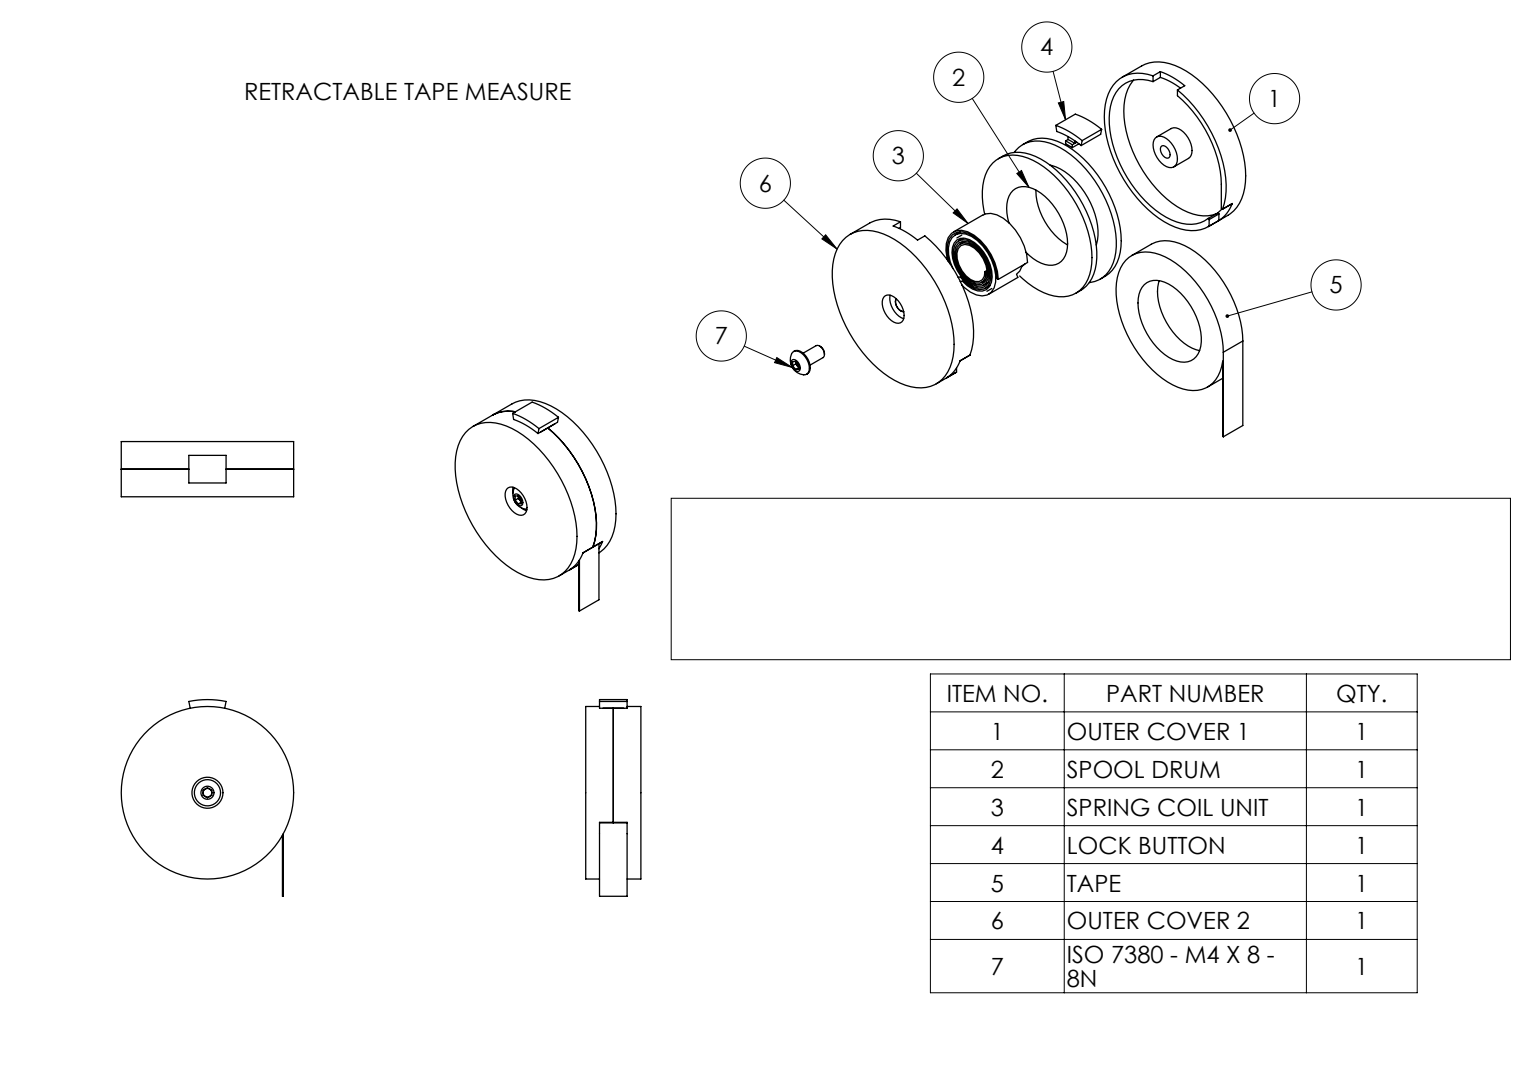
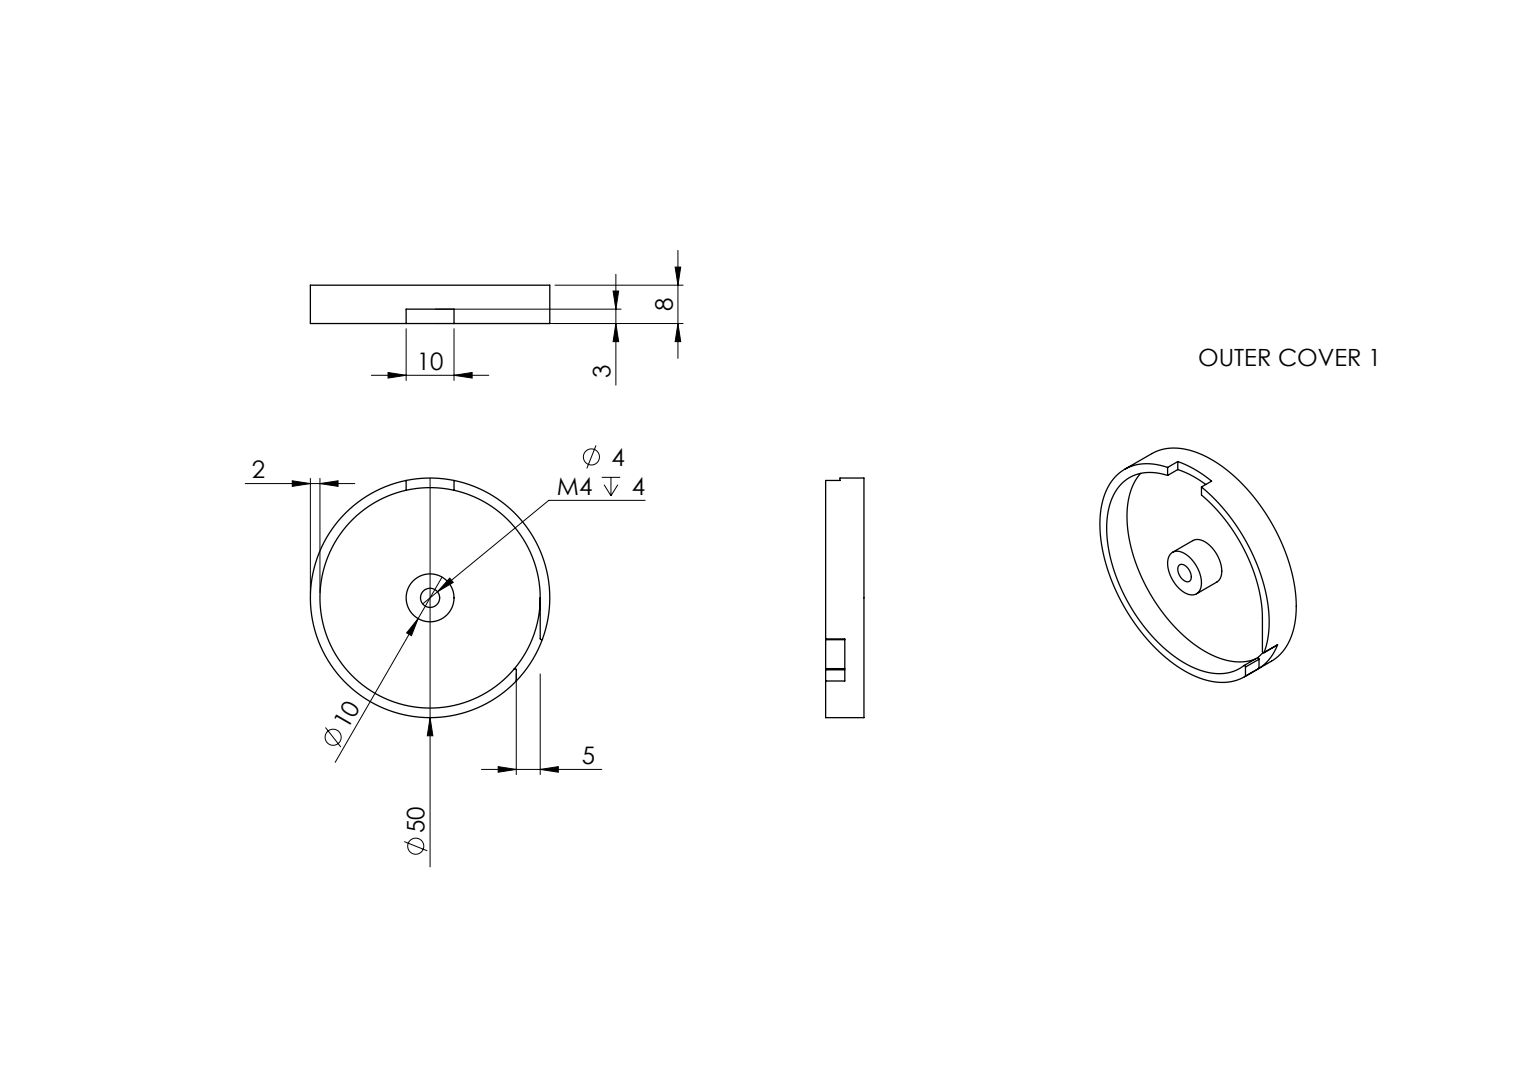
ISO-10303-21;
HEADER;
FILE_DESCRIPTION (('STEP AP214'),
    '1' );
FILE_NAME ('TAS-001',
    '2026-10-23T14:45:25',
    ( '' ),
    ( '' ),
    'SwSTEP 2.0',
    'SolidWorks 2026',
    '' );
FILE_SCHEMA (( 'AUTOMOTIVE_DESIGN' ));
ENDSEC;

DATA;
#1 = CARTESIAN_POINT ( 'NONE',  ( -5.525185448606692695, 2.707100724334796649, 1.999999999999998224 ) ) ;
#2 = DIRECTION ( 'NONE',  ( -1.000000000000000000, 0.000000000000000000, 0.000000000000000000 ) ) ;
#3 = ORIENTED_EDGE ( 'NONE', *, *, #653, .T. ) ;
#4 = EDGE_CURVE ( 'NONE', #1240, #2861, #1350, .T. ) ;
#5 = CARTESIAN_POINT ( 'NONE',  ( 10.20000000000000107, 1.971681346627238735E-16, -1.610000000000000098 ) ) ;
#6 = EDGE_CURVE ( 'NONE', #2459, #3011, #3096, .T. ) ;
#7 = CARTESIAN_POINT ( 'NONE',  ( 10.06493078320225010, 4.366638945734137245, 13.99999999999999645 ) ) ;
#8 = FILL_AREA_STYLE ('',( #407 ) ) ;
#9 = ORIENTED_EDGE ( 'NONE', *, *, #93, .F. ) ;
#10 = FACE_OUTER_BOUND ( 'NONE', #593, .T. ) ;
#11 = VERTEX_POINT ( 'NONE', #3151 ) ;
#12 = EDGE_LOOP ( 'NONE', ( #4243, #1543, #1314, #4388, #708 ) ) ;
#13 = CARTESIAN_POINT ( 'NONE',  ( 8.453438707197836521, 0.9797652757261499090, 14.00000000000000000 ) ) ;
#14 = CARTESIAN_POINT ( 'NONE',  ( 3.892125705850321804, -6.036954802193386982, 1.999999999999998224 ) ) ;
#15 = FACE_OUTER_BOUND ( 'NONE', #2318, .T. ) ;
#16 = CARTESIAN_POINT ( 'NONE',  ( 7.990059919442007441, -3.149571442993018167, 14.00000000000000000 ) ) ;
#17 = ORIENTED_EDGE ( 'NONE', *, *, #5283, .F. ) ;
#18 = CARTESIAN_POINT ( 'NONE',  ( -2.440069559021881496, 10.46881825416662259, 1.999999999999998224 ) ) ;
#19 = CARTESIAN_POINT ( 'NONE',  ( -5.000000000000085265, 24.49489742783176638, 8.000000000000000000 ) ) ;
#20 = CARTESIAN_POINT ( 'NONE',  ( 5.887534416617372202, 3.663839002572494952, 13.99999999999999645 ) ) ;
#21 = DIRECTION ( 'NONE',  ( 1.000000000000000000, 0.000000000000000000, 0.000000000000000000 ) ) ;
#22 = CARTESIAN_POINT ( 'NONE',  ( -2.415560149437878668, -8.486491385245608754, 1.999999999999998224 ) ) ;
#23 = EDGE_CURVE ( 'NONE', #5658, #4842, #4898, .T. ) ;
#24 = CARTESIAN_POINT ( 'NONE',  ( 2.877506500681688006, 7.288437455188073955, 1.999999999999998224 ) ) ;
#25 = LINE ( 'NONE', #396, #4267 ) ;
#26 = FILL_AREA_STYLE ('',( #3055 ) ) ;
#27 = DIRECTION ( 'NONE',  ( 0.000000000000000000, 0.000000000000000000, -1.000000000000000000 ) ) ;
#28 = FACE_OUTER_BOUND ( 'NONE', #3065, .T. ) ;
#29 = CARTESIAN_POINT ( 'NONE',  ( -25.00000000000000000, 0.000000000000000000, -8.000000000000000000 ) ) ;
#30 = VERTEX_POINT ( 'NONE', #94 ) ;
#31 = DIRECTION ( 'NONE',  ( -1.000000000000000000, 0.000000000000000000, 0.000000000000000000 ) ) ;
#32 = CARTESIAN_POINT ( 'NONE',  ( -10.48421140591525713, 1.206973991593908169, 13.99999999999999645 ) ) ;
#33 = AXIS2_PLACEMENT_3D ( 'NONE', #3461, #5223, #4408 ) ;
#34 = DIRECTION ( 'NONE',  ( 0.000000000000000000, 0.000000000000000000, -1.000000000000000000 ) ) ;
#35 = DIRECTION ( 'NONE',  ( 1.000000000000000000, 0.000000000000000000, -0.000000000000000000 ) ) ;
#36 = VERTEX_POINT ( 'NONE', #2452 ) ;
#37 = ORIENTED_EDGE ( 'NONE', *, *, #2017, .F. ) ;
#38 = CARTESIAN_POINT ( 'NONE',  ( -0.2798806129217078498, -8.779921314117062892, 14.00000000000000000 ) ) ;
#39 = CARTESIAN_POINT ( 'NONE',  ( 6.444084565535371567, 4.617298776321547393, 1.999999999999998224 ) ) ;
#40 = CIRCLE ( 'NONE', #4910, 25.00000000000000000 ) ;
#41 = DIRECTION ( 'NONE',  ( -0.000000000000000000, -0.000000000000000000, 1.000000000000000000 ) ) ;
#42 = CARTESIAN_POINT ( 'NONE',  ( -2.415560149437796511, -8.486491385245610530, 14.00000000000000000 ) ) ;
#43 = CIRCLE ( 'NONE', #2159, 23.00000000000000000 ) ;
#44 = ORIENTED_EDGE ( 'NONE', *, *, #3966, .F. ) ;
#45 = CARTESIAN_POINT ( 'NONE',  ( 8.595497693523489247, -5.345940745659027549, 1.999999999999998224 ) ) ;
#46 = CARTESIAN_POINT ( 'NONE',  ( -5.651290410005069376, 9.082320918485367045, 1.999999999999998224 ) ) ;
#47 =( GEOMETRIC_REPRESENTATION_CONTEXT ( 3 ) GLOBAL_UNCERTAINTY_ASSIGNED_CONTEXT ( ( #114 ) ) GLOBAL_UNIT_ASSIGNED_CONTEXT ( ( #3594, #2760, #4052 ) ) REPRESENTATION_CONTEXT ( 'NONE', 'WORKASPACE' ) );
#48 = CARTESIAN_POINT ( 'NONE',  ( -1.424809953814591523, 6.586142414399822620, 13.99999999999999645 ) ) ;
#49 = CARTESIAN_POINT ( 'NONE',  ( 7.716263785693136867, -3.801003699432787375, 1.999999999999998224 ) ) ;
#50 = CIRCLE ( 'NONE', #4195, 0.2500000000000002220 ) ;
#51 = CARTESIAN_POINT ( 'NONE',  ( 6.638644669766898154, 2.135480210976827387, 1.999999999999998224 ) ) ;
#52 = FILL_AREA_STYLE_COLOUR ( '', #5106 ) ;
#53 = DIRECTION ( 'NONE',  ( -0.000000000000000000, -0.000000000000000000, -1.000000000000000000 ) ) ;
#54 = VECTOR ( 'NONE', #1585, 1000.000000000000000 ) ;
#55 = CARTESIAN_POINT ( 'NONE',  ( 1.380000000000002336, 22.95856267278071172, 12.00000000000000000 ) ) ;
#56 = CARTESIAN_POINT ( 'NONE',  ( 2.199999999999999289, 0.000000000000000000, -3.300000000000000266 ) ) ;
#57 = CARTESIAN_POINT ( 'NONE',  ( -23.00000000000000000, 0.000000000000000000, 8.000000000000000000 ) ) ;
#58 = EDGE_LOOP ( 'NONE', ( #1044, #3800, #158, #292 ) ) ;
#59 = COLOUR_RGB ( '',0.8941176470588234615, 0.8941176470588234615, 0.8941176470588234615 ) ;
#60 = DIRECTION ( 'NONE',  ( -0.7071067811865492381, 8.659560562354911904E-17, -0.7071067811865457964 ) ) ;
#61 = CARTESIAN_POINT ( 'NONE',  ( -3.798941939731700579, -9.621416145859109648, 13.99999999999999645 ) ) ;
#62 = FILL_AREA_STYLE_COLOUR ( '', #2698 ) ;
#63 = CARTESIAN_POINT ( 'NONE',  ( -12.50000000000000000, 0.000000000000000000, 14.00000000000000000 ) ) ;
#64 = ORIENTED_EDGE ( 'NONE', *, *, #3045, .T. ) ;
#65 = ORIENTED_EDGE ( 'NONE', *, *, #4214, .F. ) ;
#66 = CARTESIAN_POINT ( 'NONE',  ( -7.161907081466633684, 5.673982509929174967, 14.00000000000000000 ) ) ;
#67 = CARTESIAN_POINT ( 'NONE',  ( 7.024953159363688471, -4.052930060063556716, 1.999999999999998224 ) ) ;
#68 = AXIS2_PLACEMENT_3D ( 'NONE', #3117, #2273, #3510 ) ;
#69 = ADVANCED_BREP_SHAPE_REPRESENTATION ( '', ( #652, #1336 ), #2338 ) ;
#70 = CARTESIAN_POINT ( 'NONE',  ( -7.550296695603107899, -2.566425989403007257, 1.999999999999998224 ) ) ;
#71 = CARTESIAN_POINT ( 'NONE',  ( 0.7514524083000287957, 9.263466152293682754, 14.00000000000000000 ) ) ;
#72 = VECTOR ( 'NONE', #3186, 1000.000000000000000 ) ;
#73 = VERTEX_POINT ( 'NONE', #3260 ) ;
#74 = CARTESIAN_POINT ( 'NONE',  ( 9.807503887220748950, -2.283819133639664489, 1.999999999999998224 ) ) ;
#75 = CARTESIAN_POINT ( 'NONE',  ( 6.160418207306094018, 1.983851483784787373, 14.00000000000000000 ) ) ;
#76 = CARTESIAN_POINT ( 'NONE',  ( -7.091148812992124739, -4.571561645351811976, 13.99999999999999645 ) ) ;
#77 = CARTESIAN_POINT ( 'NONE',  ( -8.026550172065741506, -2.724140490265046122, 13.99999999999999645 ) ) ;
#78 = ITEM_DEFINED_TRANSFORMATION ( 'NONE', 'NONE', #1407,  #1336 ) ;
#79 = CARTESIAN_POINT ( 'NONE',  ( -4.424777426321968576, -7.679192617323552739, 1.999999999999998224 ) ) ;
#80 = CARTESIAN_POINT ( 'NONE',  ( 5.887534416617370425, 3.663839002572738313, 1.999999999999998224 ) ) ;
#81 = EDGE_CURVE ( 'NONE', #5595, #92, #3920, .T. ) ;
#82 = CARTESIAN_POINT ( 'NONE',  ( -2.149999999999997691, 2.632990618166807263E-16, -8.000000000000000000 ) ) ;
#83 =( NAMED_UNIT ( * ) SI_UNIT ( $, .STERADIAN. ) SOLID_ANGLE_UNIT ( ) );
#84 = CARTESIAN_POINT ( 'NONE',  ( 1.380000000000002558, 22.95856267278071527, 1.371299631966804711 ) ) ;
#85 = DIRECTION ( 'NONE',  ( 0.000000000000000000, 0.000000000000000000, 1.000000000000000000 ) ) ;
#86 = FACE_OUTER_BOUND ( 'NONE', #1906, .T. ) ;
#87 = DIRECTION ( 'NONE',  ( 0.000000000000000000, 0.000000000000000000, -1.000000000000000000 ) ) ;
#88 = ADVANCED_FACE ( 'NONE', ( #5011, #2771 ), #1450, .T. ) ;
#89 = CARTESIAN_POINT ( 'NONE',  ( -8.483256258862985177, -6.077987531410205868, 13.99999999999999645 ) ) ;
#90 = SURFACE_SIDE_STYLE ('',( #2360 ) ) ;
#91 = DIRECTION ( 'NONE',  ( -0.000000000000000000, -0.000000000000000000, -1.000000000000000000 ) ) ;
#92 = VERTEX_POINT ( 'NONE', #1069 ) ;
#93 = EDGE_CURVE ( 'NONE', #5647, #11, #1098, .T. ) ;
#94 = CARTESIAN_POINT ( 'NONE',  ( -23.00000000000000000, 0.000000000000000000, 2.000000000000000000 ) ) ;
#95 = CARTESIAN_POINT ( 'NONE',  ( -6.708753103182797162, 7.642576097240647570, 14.00000000000000000 ) ) ;
#96 = CARTESIAN_POINT ( 'NONE',  ( 7.409328306158467825, 2.927536720054290775, 1.999999999999998224 ) ) ;
#97 = CARTESIAN_POINT ( 'NONE',  ( 5.612687125617794592, -6.603876269260512188, 1.999999999999998224 ) ) ;
#98 = CARTESIAN_POINT ( 'NONE',  ( -6.185289998984974780, -6.402116997106622520, 14.00000000000000000 ) ) ;
#99 = ORIENTED_EDGE ( 'NONE', *, *, #1510, .T. ) ;
#100 = CARTESIAN_POINT ( 'NONE',  ( -0.7077576507783156501, 10.75210906117156995, 1.999999999999998224 ) ) ;
#101 = CARTESIAN_POINT ( 'NONE',  ( 0.000000000000000000, -0.7216878364870318308, -1.250000000000000000 ) ) ;
#102 = CARTESIAN_POINT ( 'NONE',  ( 5.103689747953259470, 6.014827819656690444, 13.99999999999999645 ) ) ;
#103 = CARTESIAN_POINT ( 'NONE',  ( -8.388197440585694054, -1.387539741535495974, 13.99999999999999645 ) ) ;
#104 = CARTESIAN_POINT ( 'NONE',  ( 1.492118473828444536, -5.588909376072072277, 14.00000000000000000 ) ) ;
#105 = EDGE_CURVE ( 'NONE', #3518, #3244, #4364, .T. ) ;
#106 = CARTESIAN_POINT ( 'NONE',  ( -8.126042061586874254, 2.755650963504471473, 1.999999999999998224 ) ) ;
#107 = DIRECTION ( 'NONE',  ( -0.000000000000000000, 0.000000000000000000, 1.000000000000000000 ) ) ;
#108 = CARTESIAN_POINT ( 'NONE',  ( -0.5497243705170606898, -6.763214047005217999, 1.999999999999998224 ) ) ;
#109 = ORIENTED_EDGE ( 'NONE', *, *, #4578, .T. ) ;
#110 = DIRECTION ( 'NONE',  ( -1.000000000000000000, 0.000000000000000000, 0.000000000000000000 ) ) ;
#111 = CARTESIAN_POINT ( 'NONE',  ( 17.55913978494622896, -14.85518798308249266, 8.000000000000000000 ) ) ;
#112 = FACE_OUTER_BOUND ( 'NONE', #2425, .T. ) ;
#113 = SURFACE_STYLE_FILL_AREA ( #890 ) ;
#114 = UNCERTAINTY_MEASURE_WITH_UNIT (LENGTH_MEASURE( 1.000000000000000082E-05 ), #3594, 'distance_accuracy_value', 'NONE');
#115 = CARTESIAN_POINT ( 'NONE',  ( 5.800093669798302543, -8.375184749302979625, 13.99999999999999645 ) ) ;
#116 = DIRECTION ( 'NONE',  ( 2.385244779468107388E-15, 1.000000000000000000, 0.000000000000000000 ) ) ;
#117 = ORIENTED_EDGE ( 'NONE', *, *, #2522, .T. ) ;
#118 = VERTEX_POINT ( 'NONE', #3747 ) ;
#119 = CARTESIAN_POINT ( 'NONE',  ( -3.139313036748870189, 9.741172307225710369, 14.00000000000000000 ) ) ;
#120 = CARTESIAN_POINT ( 'NONE',  ( -0.2539011084975961174, 7.766605221862830533, 1.999999999999998224 ) ) ;
#121 = VECTOR ( 'NONE', #3967, 999.9999999999998863 ) ;
#122 = CARTESIAN_POINT ( 'NONE',  ( -8.763921109942213405, 2.343993041296470459, 1.999999999999998224 ) ) ;
#123 = CARTESIAN_POINT ( 'NONE',  ( -7.559400777704423646, -6.425066744314204215, 14.00000000000000000 ) ) ;
#124 = ADVANCED_FACE ( 'NONE', ( #4956 ), #3318, .T. ) ;
#125 = EDGE_LOOP ( 'NONE', ( #2926, #4809, #268, #1968 ) ) ;
#126 = CARTESIAN_POINT ( 'NONE',  ( 7.631804465921431913, -6.689046765414639495, 1.999999999999998224 ) ) ;
#127 = CIRCLE ( 'NONE', #405, 23.00000000000000000 ) ;
#128 = CARTESIAN_POINT ( 'NONE',  ( 22.50000000000000355, 2.755455298081545172E-15, 4.000000000000000000 ) ) ;
#129 = CARTESIAN_POINT ( 'NONE',  ( 0.5754137710878940437, 8.770917875152660415, 13.99999999999999645 ) ) ;
#130 = AXIS2_PLACEMENT_3D ( 'NONE', #3700, #1115, #2554 ) ;
#131 = CARTESIAN_POINT ( 'NONE',  ( -9.772156678340820690, -2.119544458102139206, 1.999999999999998224 ) ) ;
#132 = VERTEX_POINT ( 'NONE', #668 ) ;
#133 = CARTESIAN_POINT ( 'NONE',  ( 3.747087600548639763, -7.295897990121164689, 1.999999999999998224 ) ) ;
#134 = AXIS2_PLACEMENT_3D ( 'NONE', #4325, #5590, #2673 ) ;
#135 = AXIS2_PLACEMENT_3D ( 'NONE', #259, #5439, #1064 ) ;
#136 = PLANE ( 'NONE',  #3174 ) ;
#137 = CARTESIAN_POINT ( 'NONE',  ( -7.019651866617071079, -0.1200674265790944856, 1.999999999999998224 ) ) ;
#138 = CIRCLE ( 'NONE', #1889, 1.999999999999999112 ) ;
#139 = ORIENTED_EDGE ( 'NONE', *, *, #5614, .T. ) ;
#140 = CARTESIAN_POINT ( 'NONE',  ( -3.597458971453999066, 6.226096630968013024, 1.999999999999998224 ) ) ;
#141 = DIRECTION ( 'NONE',  ( -0.000000000000000000, -0.000000000000000000, -1.000000000000000000 ) ) ;
#142 = LINE ( 'NONE', #1986, #246 ) ;
#143 = SHAPE_REPRESENTATION ( 'Lock Button', ( #1336 ), #3242 ) ;
#144 = AXIS2_PLACEMENT_3D ( 'NONE', #2084, #4329, #2630 ) ;
#145 = LINE ( 'NONE', #1902, #3817 ) ;
#146 = DIRECTION ( 'NONE',  ( 1.000000000000000000, 0.000000000000000000, 0.000000000000000000 ) ) ;
#147 = VECTOR ( 'NONE', #3798, 1000.000000000000000 ) ;
#148 = DIRECTION ( 'NONE',  ( 0.000000000000000000, 0.000000000000000000, -1.000000000000000000 ) ) ;
#149 = EDGE_CURVE ( 'NONE', #3887, #4410, #641, .T. ) ;
#150 = ORIENTED_EDGE ( 'NONE', *, *, #4696, .T. ) ;
#151 = DIRECTION ( 'NONE',  ( 0.000000000000000000, -0.4999999999999998890, 0.8660254037844387076 ) ) ;
#152 = CARTESIAN_POINT ( 'NONE',  ( -9.772156678340820690, -2.119544458102511353, 14.00000000000000000 ) ) ;
#153 = CARTESIAN_POINT ( 'NONE',  ( 7.344045208304290639, 5.086154276871864610, 1.999999999999998224 ) ) ;
#154 = ADVANCED_FACE ( 'NONE', ( #5473 ), #2392, .F. ) ;
#155 = EDGE_CURVE ( 'NONE', #132, #1194, #1259, .T. ) ;
#156 = CARTESIAN_POINT ( 'NONE',  ( 4.415008247871750058, 7.106745273741266189, 1.999999999999998224 ) ) ;
#157 = CARTESIAN_POINT ( 'NONE',  ( -4.983290658054754019, 7.721050520723660604, 14.00000000000000000 ) ) ;
#158 = ORIENTED_EDGE ( 'NONE', *, *, #190, .T. ) ;
#159 = VECTOR ( 'NONE', #187, 1000.000000000000114 ) ;
#160 = DIRECTION ( 'NONE',  ( -1.000000000000000000, 1.156482317317871478E-16, 0.000000000000000000 ) ) ;
#161 = DIRECTION ( 'NONE',  ( -4.364351673553916694E-15, 1.000000000000000000, 0.000000000000000000 ) ) ;
#162 = CARTESIAN_POINT ( 'NONE',  ( -5.390757458300978300, 6.793134358447313836, 13.99999999999999645 ) ) ;
#163 = CIRCLE ( 'NONE', #2186, 15.00000000000000000 ) ;
#164 = CARTESIAN_POINT ( 'NONE',  ( -0.6809175113353352904, 10.25113960786383771, 1.999999999999998224 ) ) ;
#165 = ORIENTED_EDGE ( 'NONE', *, *, #624, .F. ) ;
#166 = CARTESIAN_POINT ( 'NONE',  ( 3.388254439433305176, -8.575817650944026482, 1.999999999999998224 ) ) ;
#167 = EDGE_CURVE ( 'NONE', #3046, #5218, #4525, .T. ) ;
#168 = DIRECTION ( 'NONE',  ( -1.000000000000000000, -0.000000000000000000, -0.000000000000000000 ) ) ;
#169 = FILL_AREA_STYLE ('',( #1465 ) ) ;
#170 = CARTESIAN_POINT ( 'NONE',  ( -1.320393794063943416, 6.095439640211752774, 1.999999999999998224 ) ) ;
#171 = EDGE_LOOP ( 'NONE', ( #4985, #2532, #4601, #4935, #348, #2849 ) ) ;
#172 = CARTESIAN_POINT ( 'NONE',  ( -4.975175822334872322, 5.137265612443480123, 1.999999999999998224 ) ) ;
#173 = DIRECTION ( 'NONE',  ( 1.000000000000000000, 0.000000000000000000, -0.000000000000000000 ) ) ;
#174 = DIRECTION ( 'NONE',  ( 1.000000000000000000, 0.000000000000000000, 0.000000000000000000 ) ) ;
#175 = DIRECTION ( 'NONE',  ( -0.000000000000000000, -0.000000000000000000, 1.000000000000000000 ) ) ;
#176 = CARTESIAN_POINT ( 'NONE',  ( 1.380000000000002558, 22.95856267278071527, 11.00000000000000000 ) ) ;
#177 = PRODUCT_DEFINITION ( 'UNKNOWN', '', #2504, #5623 ) ;
#178 = LINE ( 'NONE', #3662, #4829 ) ;
#179 = ORIENTED_EDGE ( 'NONE', *, *, #1806, .T. ) ;
#180 = DIRECTION ( 'NONE',  ( -0.000000000000000000, -0.000000000000000000, 1.000000000000000000 ) ) ;
#181 = CARTESIAN_POINT ( 'NONE',  ( 0.7514524083000287957, 9.263466152293682754, 14.00000000000000000 ) ) ;
#182 = CARTESIAN_POINT ( 'NONE',  ( 4.043470907200509501, 7.877814422643418801, 1.999999999999998224 ) ) ;
#183 = CARTESIAN_POINT ( 'NONE',  ( -1.480145937554574020, 8.115026467928048604, 1.999999999999998224 ) ) ;
#184 = CARTESIAN_POINT ( 'NONE',  ( 7.258279873954945671, -6.354128476750924293, 14.00000000000000000 ) ) ;
#185 = FACE_OUTER_BOUND ( 'NONE', #2391, .T. ) ;
#186 = VERTEX_POINT ( 'NONE', #5039 ) ;
#187 = DIRECTION ( 'NONE',  ( -0.000000000000000000, -0.5000000000000002220, 0.8660254037844384856 ) ) ;
#188 = CARTESIAN_POINT ( 'NONE',  ( 5.326024957120313985, -1.813589758486611858, 14.00000000000000000 ) ) ;
#189 = CARTESIAN_POINT ( 'NONE',  ( -2.179108132477381332, -10.08557389312607278, 13.99999999999999645 ) ) ;
#190 = EDGE_CURVE ( 'NONE', #442, #1012, #3278, .T. ) ;
#191 = CARTESIAN_POINT ( 'NONE',  ( 3.896371052708265559, -4.167854722423870228, 14.00000000000000000 ) ) ;
#192 = EDGE_LOOP ( 'NONE', ( #1018, #4430, #1762, #1166 ) ) ;
#193 = CARTESIAN_POINT ( 'NONE',  ( -1.063411474431080306, -9.238278818534249481, 1.999999999999998224 ) ) ;
#194 = CARTESIAN_POINT ( 'NONE',  ( -25.00000000000000000, 0.000000000000000000, -8.000000000000000000 ) ) ;
#195 = CARTESIAN_POINT ( 'NONE',  ( -6.742266116715657454, -1.811900715329134215, 1.999999999999998224 ) ) ;
#196 = ADVANCED_FACE ( 'NONE', ( #1959 ), #1125, .F. ) ;
#197 = ORIENTED_EDGE ( 'NONE', *, *, #3580, .T. ) ;
#198 = CARTESIAN_POINT ( 'NONE',  ( -6.041022033915842471, 3.753782041846908779, 1.999999999999998224 ) ) ;
#199 = CARTESIAN_POINT ( 'NONE',  ( 0.000000000000000000, 0.000000000000000000, 12.00000000000000000 ) ) ;
#200 = CARTESIAN_POINT ( 'NONE',  ( -3.379911625893651017, -5.460782782531100388, 13.99999999999999645 ) ) ;
#201 = CARTESIAN_POINT ( 'NONE',  ( 0.000000000000000000, 0.000000000000000000, 14.00000000000000000 ) ) ;
#202 = CARTESIAN_POINT ( 'NONE',  ( 25.00000000000000000, -3.061616997868383043E-15, -8.000000000000000000 ) ) ;
#203 = LINE ( 'NONE', #3710, #3455 ) ;
#204 = ORIENTED_EDGE ( 'NONE', *, *, #5079, .F. ) ;
#205 = DIRECTION ( 'NONE',  ( 1.000000000000000000, 0.000000000000000000, 0.000000000000000000 ) ) ;
#206 = PRESENTATION_LAYER_ASSIGNMENT (  '', '', ( #477 ) ) ;
#207 = DIRECTION ( 'NONE',  ( 1.000000000000000000, 0.000000000000000000, 0.000000000000000000 ) ) ;
#208 = CARTESIAN_POINT ( 'NONE',  ( -8.440272934376206848, 1.393994921405934173, 1.999999999999998224 ) ) ;
#209 = CARTESIAN_POINT ( 'NONE',  ( 4.326322805050086373, -6.952463250691143237, 13.99999999999999645 ) ) ;
#210 = CARTESIAN_POINT ( 'NONE',  ( -2.067895747887561697, -9.596367745172036834, 1.999999999999998224 ) ) ;
#211 =( GEOMETRIC_REPRESENTATION_CONTEXT ( 3 ) GLOBAL_UNCERTAINTY_ASSIGNED_CONTEXT ( ( #5230 ) ) GLOBAL_UNIT_ASSIGNED_CONTEXT ( ( #2989, #5121, #2439 ) ) REPRESENTATION_CONTEXT ( 'NONE', 'WORKASPACE' ) );
#212 = DIRECTION ( 'NONE',  ( 0.000000000000000000, 0.000000000000000000, 1.000000000000000000 ) ) ;
#213 = DIRECTION ( 'NONE',  ( 0.000000000000000000, 0.000000000000000000, -1.000000000000000000 ) ) ;
#214 = EDGE_LOOP ( 'NONE', ( #9, #1202, #2223 ) ) ;
#215 = CARTESIAN_POINT ( 'NONE',  ( 1.300000000000000044, 0.7216878364870328300, -1.250000000000000000 ) ) ;
#216 = CARTESIAN_POINT ( 'NONE',  ( -1.105557477332586691, -6.708264047591377732, 14.00000000000000000 ) ) ;
#217 = CARTESIAN_POINT ( 'NONE',  ( -8.745075223331019387, 3.959260399367729111, 13.99999999999999645 ) ) ;
#218 = CARTESIAN_POINT ( 'NONE',  ( -4.354965481614496703, -8.841480220787186539, 1.999999999999998224 ) ) ;
#219 = AXIS2_PLACEMENT_3D ( 'NONE', #5135, #3840, #5044 ) ;
#220 = ORIENTED_EDGE ( 'NONE', *, *, #4170, .T. ) ;
#221 = CARTESIAN_POINT ( 'NONE',  ( -0.1359230501497094012, -8.279147739300480424, 1.999999999999998224 ) ) ;
#222 = AXIS2_PLACEMENT_3D ( 'NONE', #3534, #53, #4345 ) ;
#223 = LINE ( 'NONE', #741, #591 ) ;
#224 = EDGE_CURVE ( 'NONE', #1931, #3723, #579, .T. ) ;
#225 =( NAMED_UNIT ( * ) PLANE_ANGLE_UNIT ( ) SI_UNIT ( $, .RADIAN. ) );
#226 = CARTESIAN_POINT ( 'NONE',  ( 2.227988792049259814, 5.923272706911028251, 1.999999999999998224 ) ) ;
#227 = ORIENTED_EDGE ( 'NONE', *, *, #1608, .T. ) ;
#228 = CARTESIAN_POINT ( 'NONE',  ( 3.520917041835318173, -6.848083076130971669, 1.999999999999998224 ) ) ;
#229 = CARTESIAN_POINT ( 'NONE',  ( 0.000000000000000000, 0.000000000000000000, 8.000000000000000000 ) ) ;
#230 = CARTESIAN_POINT ( 'NONE',  ( 1.380000000000002558, 22.95856267278071527, 11.00000000000000000 ) ) ;
#231 = CARTESIAN_POINT ( 'NONE',  ( 0.000000000000000000, 0.000000000000000000, -3.106350832689629637 ) ) ;
#232 = ORIENTED_EDGE ( 'NONE', *, *, #2358, .F. ) ;
#233 = CIRCLE ( 'NONE', #3913, 2.149999999999997691 ) ;
#234 = DIRECTION ( 'NONE',  ( 0.000000000000000000, 0.000000000000000000, 1.000000000000000000 ) ) ;
#235 = CARTESIAN_POINT ( 'NONE',  ( 0.000000000000000000, 0.000000000000000000, -8.000000000000000000 ) ) ;
#236 = CARTESIAN_POINT ( 'NONE',  ( -0.1359230501497094012, -8.279147739300480424, 1.999999999999998224 ) ) ;
#237 = CARTESIAN_POINT ( 'NONE',  ( -5.921118896519415919, 6.318058289644736369, 13.99999999999999645 ) ) ;
#238 = DIRECTION ( 'NONE',  ( -0.000000000000000000, -0.000000000000000000, -1.000000000000000000 ) ) ;
#239 = ORIENTED_EDGE ( 'NONE', *, *, #2358, .T. ) ;
#240 = CARTESIAN_POINT ( 'NONE',  ( 1.820000000000000062, 3.799999999999999378, 0.000000000000000000 ) ) ;
#241 = ORIENTED_EDGE ( 'NONE', *, *, #4606, .T. ) ;
#242 = FACE_OUTER_BOUND ( 'NONE', #323, .T. ) ;
#243 = CARTESIAN_POINT ( 'NONE',  ( 6.004028658818958419, -2.715480180205860794, 14.00000000000000000 ) ) ;
#244 = CARTESIAN_POINT ( 'NONE',  ( 3.917689075872249571, 9.035181080458080771, 13.99999999999999645 ) ) ;
#245 = CARTESIAN_POINT ( 'NONE',  ( -0.5497243705170608008, -6.763214047005219776, 14.00000000000000000 ) ) ;
#246 = VECTOR ( 'NONE', #2299, 1000.000000000000000 ) ;
#247 = VERTEX_POINT ( 'NONE', #3664 ) ;
#248 = PRODUCT_RELATED_PRODUCT_CATEGORY ( 'part', '', ( #2062 ) ) ;
#249 = CARTESIAN_POINT ( 'NONE',  ( -10.48421140591450751, 1.206973991593908169, 1.999999999999998224 ) ) ;
#250 = AXIS2_PLACEMENT_3D ( 'NONE', #4950, #1491, #1007 ) ;
#251 = ADVANCED_FACE ( 'NONE', ( #5066 ), #4211, .F. ) ;
#252 = CARTESIAN_POINT ( 'NONE',  ( 1.820000000000000062, 0.000000000000000000, 3.799999999999999378 ) ) ;
#253 = CARTESIAN_POINT ( 'NONE',  ( 6.680730669075649608, 3.301097878975988387, 1.999999999999998224 ) ) ;
#254 = ORIENTED_EDGE ( 'NONE', *, *, #1540, .F. ) ;
#255 = CARTESIAN_POINT ( 'NONE',  ( -5.416162817796314144, -4.301262981183148426, 1.999999999999998224 ) ) ;
#256 = CARTESIAN_POINT ( 'NONE',  ( -2.466819000628106551, 6.242838961510105200, 1.999999999999998224 ) ) ;
#257 = EDGE_CURVE ( 'NONE', #4241, #4349, #3460, .T. ) ;
#258 = CARTESIAN_POINT ( 'NONE',  ( 4.793600759081160234, 4.956424179878266223, 13.99999999999999645 ) ) ;
#259 = CARTESIAN_POINT ( 'NONE',  ( 17.74999999999999289, -15.01665741768121443, 8.000000000000000000 ) ) ;
#260 = CARTESIAN_POINT ( 'NONE',  ( 9.809999999999998721, 0.000000000000000000, 0.000000000000000000 ) ) ;
#261 = VERTEX_POINT ( 'NONE', #4126 ) ;
#262 = CARTESIAN_POINT ( 'NONE',  ( 0.000000000000000000, 0.000000000000000000, 8.000000000000000000 ) ) ;
#263 = FACE_OUTER_BOUND ( 'NONE', #5640, .T. ) ;
#264 = CARTESIAN_POINT ( 'NONE',  ( 3.747087600548639763, -7.295897990121164689, 1.999999999999998224 ) ) ;
#265 = CARTESIAN_POINT ( 'NONE',  ( -7.364573508975984062, 1.714675912027187943, 13.99999999999999645 ) ) ;
#266 = CARTESIAN_POINT ( 'NONE',  ( 5.030817567586885808, 9.062633982223131213, 14.00000000000000000 ) ) ;
#267 = EDGE_CURVE ( 'NONE', #1755, #5130, #3687, .T. ) ;
#268 = ORIENTED_EDGE ( 'NONE', *, *, #1278, .T. ) ;
#269 = PRODUCT_DEFINITION_SHAPE ( 'NONE', 'NONE',  #3907 ) ;
#270 = DIRECTION ( 'NONE',  ( -0.000000000000000000, 0.000000000000000000, 1.000000000000000000 ) ) ;
#271 = EDGE_LOOP ( 'NONE', ( #2578, #2682 ) ) ;
#272 = DIRECTION ( 'NONE',  ( 0.000000000000000000, 0.000000000000000000, 1.000000000000000000 ) ) ;
#273 = CARTESIAN_POINT ( 'NONE',  ( -2.717942380035140992, -6.274577315194989957, 14.00000000000000000 ) ) ;
#274 = CARTESIAN_POINT ( 'NONE',  ( -1.592064345877354903, 9.625584969239746158, 13.99999999999999645 ) ) ;
#275 = CARTESIAN_POINT ( 'NONE',  ( 4.290186206382709422, 5.996800006796702220, 14.00000000000000000 ) ) ;
#276 = VERTEX_POINT ( 'NONE', #4778 ) ;
#277 = CARTESIAN_POINT ( 'NONE',  ( 7.631804465921431913, -6.689046765414639495, 1.999999999999998224 ) ) ;
#278 = FACE_OUTER_BOUND ( 'NONE', #3102, .T. ) ;
#279 = DIRECTION ( 'NONE',  ( 0.000000000000000000, 0.000000000000000000, 1.000000000000000000 ) ) ;
#280 = CARTESIAN_POINT ( 'NONE',  ( -7.652305818843809782, 2.590529227167489790, 1.999999999999998224 ) ) ;
#281 = CARTESIAN_POINT ( 'NONE',  ( 21.74999999999999645, -30.00000000000000000, 4.000000000000001776 ) ) ;
#282 = CARTESIAN_POINT ( 'NONE',  ( -1.189470317277863565, -7.202885406307538041, 13.99999999999999645 ) ) ;
#283 = CARTESIAN_POINT ( 'NONE',  ( 0.000000000000000000, 0.000000000000000000, 0.000000000000000000 ) ) ;
#284 = CARTESIAN_POINT ( 'NONE',  ( -5.000000000000000000, 0.000000000000000000, -2.000000000000000000 ) ) ;
#285 = DIRECTION ( 'NONE',  ( -0.000000000000000000, -0.000000000000000000, 1.000000000000000000 ) ) ;
#286 = VERTEX_POINT ( 'NONE', #2592 ) ;
#287 = CARTESIAN_POINT ( 'NONE',  ( 0.000000000000000000, 0.000000000000000000, -8.000000000000000000 ) ) ;
#288 = DIRECTION ( 'NONE',  ( 0.000000000000000000, 0.000000000000000000, 1.000000000000000000 ) ) ;
#289 = CARTESIAN_POINT ( 'NONE',  ( -8.017392084630253990, -4.988806607527433989, 1.999999999999998224 ) ) ;
#290 = CARTESIAN_POINT ( 'NONE',  ( 8.697835924490034287, 4.836984431370582982, 13.99999999999999645 ) ) ;
#291 = CARTESIAN_POINT ( 'NONE',  ( 9.925004466819306259, 3.374327561486830440, 14.00000000000000000 ) ) ;
#292 = ORIENTED_EDGE ( 'NONE', *, *, #2127, .F. ) ;
#293 = LINE ( 'NONE', #4272, #2527 ) ;
#294 = ORIENTED_EDGE ( 'NONE', *, *, #155, .F. ) ;
#295 = DIRECTION ( 'NONE',  ( -0.2000000000000000111, 0.9797958971132711969, 0.000000000000000000 ) ) ;
#296 = CARTESIAN_POINT ( 'NONE',  ( -5.034899347480884302, -4.722558430572732391, 14.00000000000000000 ) ) ;
#297 = CARTESIAN_POINT ( 'NONE',  ( 5.099673838353210975, -8.834479793763010846, 13.99999999999999645 ) ) ;
#298 = PRODUCT_DEFINITION_FORMATION_WITH_SPECIFIED_SOURCE ( 'ANY', '', #4227, .NOT_KNOWN. ) ;
#299 = CARTESIAN_POINT ( 'NONE',  ( 7.439669587982604249, 0.9822684312230363091, 14.00000000000000000 ) ) ;
#300 = VERTEX_POINT ( 'NONE', #812 ) ;
#301 = CARTESIAN_POINT ( 'NONE',  ( -8.017392084630253990, -4.988806607527433989, 1.999999999999998224 ) ) ;
#302 = PLANE ( 'NONE',  #1328 ) ;
#303 = VECTOR ( 'NONE', #5105, 1000.000000000000000 ) ;
#304 = CARTESIAN_POINT ( 'NONE',  ( 0.000000000000000000, 0.000000000000000000, 0.000000000000000000 ) ) ;
#305 = CARTESIAN_POINT ( 'NONE',  ( 6.929006764466009827, 4.804313515625705300, 1.999999999999998224 ) ) ;
#306 = ADVANCED_FACE ( 'NONE', ( #5530 ), #1618, .T. ) ;
#307 = CARTESIAN_POINT ( 'NONE',  ( 4.243312049792013596, -4.537448458213932945, 1.999999999999998224 ) ) ;
#308 = CARTESIAN_POINT ( 'NONE',  ( -7.375360291558942905, -1.341686286798741357, 13.99999999999999645 ) ) ;
#309 = AXIS2_PLACEMENT_3D ( 'NONE', #1717, #5231, #3017 ) ;
#310 =( LENGTH_UNIT ( ) NAMED_UNIT ( * ) SI_UNIT ( .MILLI., .METRE. ) );
#311 = CARTESIAN_POINT ( 'NONE',  ( -4.354965481614496703, -8.841480220787186539, 1.999999999999998224 ) ) ;
#312 = ADVANCED_FACE ( 'NONE', ( #3377 ), #4350, .T. ) ;
#313 = DIRECTION ( 'NONE',  ( 0.000000000000000000, 0.000000000000000000, -1.000000000000000000 ) ) ;
#314 =( LENGTH_UNIT ( ) NAMED_UNIT ( * ) SI_UNIT ( .MILLI., .METRE. ) );
#315 = ORIENTED_EDGE ( 'NONE', *, *, #1380, .F. ) ;
#316 = PLANE ( 'NONE',  #4655 ) ;
#317 = CARTESIAN_POINT ( 'NONE',  ( 21.74999999999999645, -30.00000000000000000, 4.000000000000001776 ) ) ;
#318 = AXIS2_PLACEMENT_3D ( 'NONE', #1588, #1158, #4183 ) ;
#319 = EDGE_CURVE ( 'NONE', #2874, #3841, #1900, .T. ) ;
#320 = CARTESIAN_POINT ( 'NONE',  ( 6.971023843911450690, -5.915260676233724091, 13.99999999999999645 ) ) ;
#321 = CARTESIAN_POINT ( 'NONE',  ( 8.774740126074163982, 5.663528079765788981, 14.00000000000000000 ) ) ;
#323 = EDGE_LOOP ( 'NONE', ( #4810, #3958, #689, #578, #1562 ) ) ;
#322 = AXIS2_PLACEMENT_3D ( 'NONE', #2249, #3206, #3094 ) ;
#324 = DIRECTION ( 'NONE',  ( -0.9797958971132711969, 0.2000000000000004552, 0.000000000000000000 ) ) ;
#325 = ORIENTED_EDGE ( 'NONE', *, *, #4902, .F. ) ;
#326 = LINE ( 'NONE', #2542, #614 ) ;
#327 = CARTESIAN_POINT ( 'NONE',  ( -6.334648143026945455, -2.872559841354017429, 14.00000000000000000 ) ) ;
#328 = EDGE_CURVE ( 'NONE', #3244, #3518, #3734, .T. ) ;
#329 = CARTESIAN_POINT ( 'NONE',  ( 10.40193138080327628, 3.529992181067589829, 13.99999999999999645 ) ) ;
#330 = AXIS2_PLACEMENT_3D ( 'NONE', #260, #4634, #2330 ) ;
#331 = VECTOR ( 'NONE', #2830, 1000.000000000000114 ) ;
#332 = CARTESIAN_POINT ( 'NONE',  ( 4.443413384189735638, 4.597174039215665253, 14.00000000000000000 ) ) ;
#333 = ORIENTED_EDGE ( 'NONE', *, *, #340, .F. ) ;
#334 = CIRCLE ( 'NONE', #715, 2.149999999999997691 ) ;
#335 = CARTESIAN_POINT ( 'NONE',  ( 9.807503887220748950, -2.283819133639664489, 1.999999999999998224 ) ) ;
#336 = CARTESIAN_POINT ( 'NONE',  ( 0.000000000000000000, 0.000000000000000000, 4.000000000000000000 ) ) ;
#337 = MECHANICAL_DESIGN_GEOMETRIC_PRESENTATION_REPRESENTATION (  '', ( #5488 ), #5215 ) ;
#338 = DIRECTION ( 'NONE',  ( 1.000000000000000000, 0.000000000000000000, 0.000000000000000000 ) ) ;
#339 = CARTESIAN_POINT ( 'NONE',  ( 6.037635170864973588, 5.848285684830694997, 1.999999999999998224 ) ) ;
#340 = EDGE_CURVE ( 'NONE', #1755, #3088, #1648, .T. ) ;
#341 = DIRECTION ( 'NONE',  ( -0.000000000000000000, -0.000000000000000000, 1.000000000000000000 ) ) ;
#342 = CIRCLE ( 'NONE', #3844, 5.000000000000000000 ) ;
#343 = CARTESIAN_POINT ( 'NONE',  ( 6.997680802075244344, 0.4609939245309428446, 13.99999999999999645 ) ) ;
#344 = CARTESIAN_POINT ( 'NONE',  ( -9.772156678340820690, -2.119544458102139206, 1.999999999999998224 ) ) ;
#345 = CIRCLE ( 'NONE', #3293, 1.249999999999999778 ) ;
#346 = DIRECTION ( 'NONE',  ( 0.000000000000000000, 0.000000000000000000, -1.000000000000000000 ) ) ;
#347 = CARTESIAN_POINT ( 'NONE',  ( 2.149999999999997691, 0.000000000000000000, -8.000000000000000000 ) ) ;
#348 = ORIENTED_EDGE ( 'NONE', *, *, #1101, .F. ) ;
#349 = DIRECTION ( 'NONE',  ( 0.000000000000000000, 0.000000000000000000, 1.000000000000000000 ) ) ;
#350 = CARTESIAN_POINT ( 'NONE',  ( 1.300000000000000044, -1.082531754730548412, 0.6249999999999998890 ) ) ;
#351 = CARTESIAN_POINT ( 'NONE',  ( 2.701324588234351953, 8.405562337868641265, 13.99999999999999645 ) ) ;
#352 = EDGE_CURVE ( 'NONE', #3586, #36, #4839, .T. ) ;
#353 = CARTESIAN_POINT ( 'NONE',  ( 23.00000000000000000, -2.816687638038912352E-15, -8.000000000000000000 ) ) ;
#354 = VERTEX_POINT ( 'NONE', #2939 ) ;
#355 = DIRECTION ( 'NONE',  ( -0.000000000000000000, -0.000000000000000000, 1.000000000000000000 ) ) ;
#356 = ORIENTED_EDGE ( 'NONE', *, *, #916, .T. ) ;
#357 = DIRECTION ( 'NONE',  ( -1.000000000000000000, 0.000000000000000000, 0.000000000000000000 ) ) ;
#358 = CARTESIAN_POINT ( 'NONE',  ( 8.156937663706065322, 2.333191796391004047, 14.00000000000000000 ) ) ;
#359 = CARTESIAN_POINT ( 'NONE',  ( -7.945634105012030268, -6.745245841439798440, 13.99999999999999645 ) ) ;
#360 = CARTESIAN_POINT ( 'NONE',  ( 10.20000000000000107, 0.000000000000000000, 0.000000000000000000 ) ) ;
#361 = CARTESIAN_POINT ( 'NONE',  ( 6.523553822664519330, -0.1051741892335816969, 14.00000000000000000 ) ) ;
#362 = EDGE_LOOP ( 'NONE', ( #3338, #2305, #826, #2887 ) ) ;
#363 = CARTESIAN_POINT ( 'NONE',  ( -4.581738566658409617, -9.288989786611782762, 1.999999999999998224 ) ) ;
#364 = EDGE_CURVE ( 'NONE', #1139, #4301, #2266, .T. ) ;
#365 = CARTESIAN_POINT ( 'NONE',  ( -5.623512120026317618, -3.262381593763366450, 13.99999999999999645 ) ) ;
#366 = CARTESIAN_POINT ( 'NONE',  ( 7.097632634466812362, -2.668286824979932970, 1.999999999999998224 ) ) ;
#367 = CARTESIAN_POINT ( 'NONE',  ( 17.74999999999999289, -15.01665741768121443, 8.000000000000000000 ) ) ;
#368 = CARTESIAN_POINT ( 'NONE',  ( 5.586635445632386343, -4.430858740432560339, 13.99999999999999645 ) ) ;
#369 = CARTESIAN_POINT ( 'NONE',  ( -8.332455577110955858, 5.761155596213678010, 1.999999999999998224 ) ) ;
#370 = FACE_OUTER_BOUND ( 'NONE', #4591, .T. ) ;
#371 = CARTESIAN_POINT ( 'NONE',  ( 2.200000000000000178, 0.000000000000000000, 3.799999999999999378 ) ) ;
#372 = ORIENTED_EDGE ( 'NONE', *, *, #2730, .T. ) ;
#373 = DIRECTION ( 'NONE',  ( -0.000000000000000000, -0.000000000000000000, 1.000000000000000000 ) ) ;
#374 = DIRECTION ( 'NONE',  ( -3.540989467475305966E-16, -1.000000000000000000, 0.000000000000000000 ) ) ;
#375 = CARTESIAN_POINT ( 'NONE',  ( -0.7976699882156008670, 9.736979168371714621, 13.99999999999999645 ) ) ;
#376 = PLANE ( 'NONE',  #33 ) ;
#377 = ORIENTED_EDGE ( 'NONE', *, *, #2965, .T. ) ;
#378 = DIRECTION ( 'NONE',  ( -0.2000000000000004552, -0.9797958971132711969, 0.000000000000000000 ) ) ;
#379 = ORIENTED_EDGE ( 'NONE', *, *, #1622, .F. ) ;
#380 = DIRECTION ( 'NONE',  ( 0.000000000000000000, 0.000000000000000000, 1.000000000000000000 ) ) ;
#381 = CARTESIAN_POINT ( 'NONE',  ( -7.550296695602809471, -2.566425989403007257, 14.00000000000000000 ) ) ;
#382 = CARTESIAN_POINT ( 'NONE',  ( 1.869626052002579808, 6.555486721476420087, 1.999999999999998224 ) ) ;
#383 = ADVANCED_FACE ( 'NONE', ( #753 ), #4691, .T. ) ;
#384 = PRODUCT_DEFINITION_CONTEXT ( 'detailed design', #596, 'design' ) ;
#385 = LINE ( 'NONE', #4762, #4365 ) ;
#386 = CARTESIAN_POINT ( 'NONE',  ( -6.453089103408906624, 4.947336467533685500, 14.00000000000000000 ) ) ;
#387 = ORIENTED_EDGE ( 'NONE', *, *, #3947, .T. ) ;
#388 = FACE_OUTER_BOUND ( 'NONE', #4673, .T. ) ;
#389 = PRODUCT_DEFINITION_FORMATION_WITH_SPECIFIED_SOURCE ( 'ANY', '', #4589, .NOT_KNOWN. ) ;
#390 = CARTESIAN_POINT ( 'NONE',  ( 5.213743241621229707, -4.883528188333805531, 13.99999999999999645 ) ) ;
#391 = PRODUCT_CONTEXT ( 'NONE', #2359, 'mechanical' ) ;
#392 = CARTESIAN_POINT ( 'NONE',  ( -8.999716648909558359, -0.5976852874978595409, 1.999999999999998224 ) ) ;
#393 = CARTESIAN_POINT ( 'NONE',  ( 5.103689747953258582, 6.014827819656408892, 1.999999999999998224 ) ) ;
#394 = CARTESIAN_POINT ( 'NONE',  ( 7.024953159363689359, -4.052930060063556716, 13.99999999999999645 ) ) ;
#395 = EDGE_CURVE ( 'NONE', #92, #5595, #4012, .T. ) ;
#396 = CARTESIAN_POINT ( 'NONE',  ( 22.00000000000000000, 0.000000000000000000, 4.000000000000001776 ) ) ;
#397 =( LENGTH_UNIT ( ) NAMED_UNIT ( * ) SI_UNIT ( .MILLI., .METRE. ) );
#398 = ADVANCED_FACE ( 'NONE', ( #2533 ), #316, .T. ) ;
#399 = CARTESIAN_POINT ( 'NONE',  ( -8.072272399572318236, -5.790267008923112080, 1.999999999999998224 ) ) ;
#400 = DIRECTION ( 'NONE',  ( -0.000000000000000000, -0.000000000000000000, -1.000000000000000000 ) ) ;
#401 = CIRCLE ( 'NONE', #1231, 25.00000000000000000 ) ;
#402 = DIRECTION ( 'NONE',  ( -1.000000000000000000, 0.000000000000000000, 0.000000000000000000 ) ) ;
#403 = VERTEX_POINT ( 'NONE', #4665 ) ;
#404 = DIRECTION ( 'NONE',  ( 0.000000000000000000, 0.000000000000000000, 1.000000000000000000 ) ) ;
#405 = AXIS2_PLACEMENT_3D ( 'NONE', #490, #1846, #5415 ) ;
#406 = CARTESIAN_POINT ( 'NONE',  ( 8.640499015841685448, 2.466831329604985079, 13.99999999999999645 ) ) ;
#407 = FILL_AREA_STYLE_COLOUR ( '', #2056 ) ;
#408 = ORIENTED_EDGE ( 'NONE', *, *, #937, .F. ) ;
#409 = PRODUCT_DEFINITION_SHAPE ( 'NONE', 'NONE',  #1447 ) ;
#410 = CARTESIAN_POINT ( 'NONE',  ( 17.99999999999999289, -15.01665741768121443, -4.000000000000000000 ) ) ;
#411 = ORIENTED_EDGE ( 'NONE', *, *, #2956, .T. ) ;
#412 = EDGE_CURVE ( 'NONE', #4755, #1305, #3551, .T. ) ;
#413 = DIRECTION ( 'NONE',  ( 0.000000000000000000, 0.000000000000000000, -1.000000000000000000 ) ) ;
#414 = AXIS2_PLACEMENT_3D ( 'NONE', #201, #3683, #2416 ) ;
#415 = CARTESIAN_POINT ( 'NONE',  ( 5.528193227149303723, 6.314447692498919018, 14.00000000000000000 ) ) ;
#416 = CARTESIAN_POINT ( 'NONE',  ( -9.197478219253614640, 5.306711421960436326, 13.99999999999999645 ) ) ;
#417 = AXIS2_PLACEMENT_3D ( 'NONE', #1217, #3404, #5182 ) ;
#418 = DIRECTION ( 'NONE',  ( -0.000000000000000000, -0.000000000000000000, 1.000000000000000000 ) ) ;
#419 = CARTESIAN_POINT ( 'NONE',  ( 1.760389272475214373, -7.536528230137969686, 14.00000000000000000 ) ) ;
#420 = ORIENTED_EDGE ( 'NONE', *, *, #5372, .T. ) ;
#421 = CARTESIAN_POINT ( 'NONE',  ( -997.9783121635130101, 0.000000000000000000, 0.000000000000000000 ) ) ;
#422 = CONICAL_SURFACE ( 'NONE', #2718, 1.610000000000000098, 0.7853981633974458365 ) ;
#423 = CARTESIAN_POINT ( 'NONE',  ( -3.379911625893651017, -5.460782782531100388, 13.99999999999999645 ) ) ;
#424 = APPLICATION_PROTOCOL_DEFINITION ( 'draft international standard', 'automotive_design', 1998, #596 ) ;
#425 = CARTESIAN_POINT ( 'NONE',  ( -6.700137237869126849, -5.881230172875862472, 1.999999999999998224 ) ) ;
#426 = AXIS2_PLACEMENT_3D ( 'NONE', #2854, #1529, #4607 ) ;
#427 = ORIENTED_EDGE ( 'NONE', *, *, #2908, .T. ) ;
#428 = CARTESIAN_POINT ( 'NONE',  ( -5.402835942920797940, -5.063607225391133504, 1.999999999999998224 ) ) ;
#429 = EDGE_CURVE ( 'NONE', #1326, #5392, #2179, .T. ) ;
#430 = DIRECTION ( 'NONE',  ( -1.000000000000000000, -0.000000000000000000, -0.000000000000000000 ) ) ;
#431 =( NAMED_UNIT ( * ) SI_UNIT ( $, .STERADIAN. ) SOLID_ANGLE_UNIT ( ) );
#432 = DIRECTION ( 'NONE',  ( 1.000000000000000000, 4.364351673553916694E-15, 0.000000000000000000 ) ) ;
#433 = COLOUR_RGB ( '',1.000000000000000000, 0.9490196078431372140, 0.9098039215686274384 ) ;
#434 = PLANE ( 'NONE',  #1688 ) ;
#435 = CARTESIAN_POINT ( 'NONE',  ( 0.000000000000000000, 21.95856267278071527, 4.000000000000000000 ) ) ;
#436 = ORIENTED_EDGE ( 'NONE', *, *, #1530, .T. ) ;
#437 = LINE ( 'NONE', #5272, #4474 ) ;
#438 = VECTOR ( 'NONE', #2, 1000.000000000000000 ) ;
#439 = CARTESIAN_POINT ( 'NONE',  ( -7.945634105012030268, -6.745245841439798440, 13.99999999999999645 ) ) ;
#440 = ORIENTED_EDGE ( 'NONE', *, *, #5176, .T. ) ;
#441 = DIRECTION ( 'NONE',  ( 0.000000000000000000, 0.000000000000000000, 1.000000000000000000 ) ) ;
#442 = VERTEX_POINT ( 'NONE', #2044 ) ;
#443 = EDGE_LOOP ( 'NONE', ( #3408, #675, #377, #4015 ) ) ;
#444 = CARTESIAN_POINT ( 'NONE',  ( -8.547479018125100581, -2.754496926847988636, 14.00000000000000000 ) ) ;
#445 = CARTESIAN_POINT ( 'NONE',  ( -3.379911625893426308, -5.460782782531098611, 1.999999999999998224 ) ) ;
#446 = EDGE_CURVE ( 'NONE', #5376, #2874, #4836, .T. ) ;
#447 = DIRECTION ( 'NONE',  ( 1.000000000000000000, 0.000000000000000000, 0.000000000000000000 ) ) ;
#448 = CARTESIAN_POINT ( 'NONE',  ( 2.369394374793903246, -7.353877281245580377, 14.00000000000000000 ) ) ;
#449 = ORIENTED_EDGE ( 'NONE', *, *, #2127, .T. ) ;
#450 = CARTESIAN_POINT ( 'NONE',  ( 10.86297249782008123, 1.796588950249126349, 1.999999999999998224 ) ) ;
#451 = CARTESIAN_POINT ( 'NONE',  ( 6.804422688527093754, 1.586354726854036112, 13.99999999999999645 ) ) ;
#452 = APPLICATION_PROTOCOL_DEFINITION ( 'draft international standard', 'automotive_design', 1998, #2662 ) ;
#453 = CARTESIAN_POINT ( 'NONE',  ( -1.001529162299556797, -8.740421795711002417, 1.999999999999998224 ) ) ;
#454 = CARTESIAN_POINT ( 'NONE',  ( 6.460119401626724489, -2.924461030940388895, 1.999999999999998224 ) ) ;
#455 = CARTESIAN_POINT ( 'NONE',  ( 5.000000000000000000, 5.000000000000022204, 5.000000000000000000 ) ) ;
#456 = SURFACE_SIDE_STYLE ('',( #113 ) ) ;
#457 = FACE_OUTER_BOUND ( 'NONE', #2345, .T. ) ;
#458 = CARTESIAN_POINT ( 'NONE',  ( 3.622712361020122618, 5.236663886535374957, 1.999999999999998224 ) ) ;
#459 = LINE ( 'NONE', #4920, #1265 ) ;
#460 = ORIENTED_EDGE ( 'NONE', *, *, #4224, .T. ) ;
#461 = CARTESIAN_POINT ( 'NONE',  ( -5.000000000000000000, 0.000000000000000000, 2.000000000000000000 ) ) ;
#462 = CARTESIAN_POINT ( 'NONE',  ( -8.741731599017841248, 6.051300285686072478, 13.99999999999999645 ) ) ;
#463 = CARTESIAN_POINT ( 'NONE',  ( -5.000000000000076383, 22.44994432064363110, -8.000000000000000000 ) ) ;
#464 = CARTESIAN_POINT ( 'NONE',  ( 0.000000000000000000, 0.000000000000000000, 14.00000000000000000 ) ) ;
#465 = VERTEX_POINT ( 'NONE', #2969 ) ;
#466 = ORIENTED_EDGE ( 'NONE', *, *, #2118, .T. ) ;
#467 = CARTESIAN_POINT ( 'NONE',  ( -6.453089103408906624, 4.947336467533685500, 14.00000000000000000 ) ) ;
#468 = CARTESIAN_POINT ( 'NONE',  ( 2.877506500681688006, 7.288437455188073955, 1.999999999999998224 ) ) ;
#469 = DIRECTION ( 'NONE',  ( 0.000000000000000000, -0.000000000000000000, 1.000000000000000000 ) ) ;
#470 = CARTESIAN_POINT ( 'NONE',  ( 7.311638624438943523, 4.225618826270838291, 14.00000000000000000 ) ) ;
#471 = ORIENTED_EDGE ( 'NONE', *, *, #3814, .F. ) ;
#472 = CARTESIAN_POINT ( 'NONE',  ( -6.726831604608804582, -7.927219868180728213, 1.999999999999998224 ) ) ;
#473 = CARTESIAN_POINT ( 'NONE',  ( 0.000000000000000000, 0.000000000000000000, 2.000000000000000000 ) ) ;
#474 = CARTESIAN_POINT ( 'NONE',  ( 1.500000000000003109, 24.95495942693557012, 11.00000000000000000 ) ) ;
#475 = APPLICATION_PROTOCOL_DEFINITION ( 'draft international standard', 'automotive_design', 1998, #2768 ) ;
#476 = CARTESIAN_POINT ( 'NONE',  ( 3.433597602020624251, -9.098706718023301221, 1.999999999999998224 ) ) ;
#477 = STYLED_ITEM ( 'NONE', ( #1639 ), #622 ) ;
#478 = CARTESIAN_POINT ( 'NONE',  ( -7.227555219266156072, -1.939125212622417660, 1.999999999999998224 ) ) ;
#479 = DIRECTION ( 'NONE',  ( 1.000000000000000000, 0.000000000000000000, 0.000000000000000000 ) ) ;
#480 = CARTESIAN_POINT ( 'NONE',  ( 5.000000000000000000, -6.123233995736766282E-16, -8.000000000000000000 ) ) ;
#481 = ADVANCED_FACE ( 'NONE', ( #4717 ), #2104, .T. ) ;
#482 = CARTESIAN_POINT ( 'NONE',  ( 2.389076732465379216, -5.237771676861643577, 1.999999999999998224 ) ) ;
#483 = CARTESIAN_POINT ( 'NONE',  ( -5.021280548121167975, 3.603657539922314967, 2.000000000001176392 ) ) ;
#484 = DIRECTION ( 'NONE',  ( 0.000000000000000000, 0.000000000000000000, -1.000000000000000000 ) ) ;
#485 = ORIENTED_EDGE ( 'NONE', *, *, #2804, .F. ) ;
#486 = DIRECTION ( 'NONE',  ( 1.000000000000000000, -2.385244779468107388E-15, 0.000000000000000000 ) ) ;
#487 = CARTESIAN_POINT ( 'NONE',  ( 2.803319092186594474, 10.45862564946370021, 13.99999999999999645 ) ) ;
#488 = ADVANCED_FACE ( 'NONE', ( #1241, #3003 ), #4748, .T. ) ;
#489 = CIRCLE ( 'NONE', #219, 25.00000000000000355 ) ;
#490 = CARTESIAN_POINT ( 'NONE',  ( 0.000000000000000000, 0.000000000000000000, -4.000000000000000000 ) ) ;
#491 = LINE ( 'NONE', #4006, #5389 ) ;
#492 = ORIENTED_EDGE ( 'NONE', *, *, #2197, .F. ) ;
#493 = ORIENTED_EDGE ( 'NONE', *, *, #4312, .F. ) ;
#494 = CARTESIAN_POINT ( 'NONE',  ( 3.713512749563263604, 8.576920285551967282, 14.00000000000000000 ) ) ;
#495 = CARTESIAN_POINT ( 'NONE',  ( 7.761517335261689965, -2.213789340049559407, 1.999999999999998224 ) ) ;
#496 = AXIS2_PLACEMENT_3D ( 'NONE', #3912, #833, #2699 ) ;
#497 = CARTESIAN_POINT ( 'NONE',  ( -6.453089103408601090, 4.947336467533990145, 1.999999999999998224 ) ) ;
#498 = CARTESIAN_POINT ( 'NONE',  ( -3.391372024942433949, 7.476497417048839189, 14.00000000000000000 ) ) ;
#499 = AXIS2_PLACEMENT_3D ( 'NONE', #336, #5518, #5170 ) ;
#500 = EDGE_CURVE ( 'NONE', #1550, #3604, #3484, .T. ) ;
#501 = EDGE_LOOP ( 'NONE', ( #1369, #4531 ) ) ;
#502 = CARTESIAN_POINT ( 'NONE',  ( 9.077580196902394150, 4.112174628513753483, 1.999999999999998224 ) ) ;
#503 = CARTESIAN_POINT ( 'NONE',  ( -2.283612537812034216, 5.775797914528924437, 14.00000000000000000 ) ) ;
#504 = CARTESIAN_POINT ( 'NONE',  ( -8.026550172065741506, -2.724140490265046122, 13.99999999999999645 ) ) ;
#505 = VECTOR ( 'NONE', #782, 1000.000000000000000 ) ;
#506 = CARTESIAN_POINT ( 'NONE',  ( 2.877506500681688895, 7.288437455188075731, 13.99999999999999645 ) ) ;
#507 = ITEM_DEFINED_TRANSFORMATION ( 'NONE', 'NONE', #573,  #1336 ) ;
#508 = CARTESIAN_POINT ( 'NONE',  ( -9.031632682309719939, 0.1436733667526190195, 1.999999999999998224 ) ) ;
#509 = ADVANCED_FACE ( 'NONE', ( #3541 ), #2245, .F. ) ;
#510 = CLOSED_SHELL ( 'NONE', ( #4640, #572, #825, #4442, #4161, #3825 ) ) ;
#511 = VECTOR ( 'NONE', #2427, 1000.000000000000000 ) ;
#512 = CARTESIAN_POINT ( 'NONE',  ( 7.937472058416057408, 1.044590838406009414, 1.999999999999998224 ) ) ;
#513 = CARTESIAN_POINT ( 'NONE',  ( 6.000000000000000000, 0.000000000000000000, 1.999999999999998224 ) ) ;
#514 = DIRECTION ( 'NONE',  ( -1.156482317317871478E-16, -1.000000000000000000, 0.000000000000000000 ) ) ;
#515 = AXIS2_PLACEMENT_3D ( 'NONE', #5037, #699, #4209 ) ;
#516 = CARTESIAN_POINT ( 'NONE',  ( -5.000000000000076383, 22.44994432064363110, 5.000000000000000000 ) ) ;
#517 = EDGE_CURVE ( 'NONE', #3462, #3841, #3089, .T. ) ;
#518 = CARTESIAN_POINT ( 'NONE',  ( -3.595699629853521984, 5.016010494498948091, 1.999999999999998224 ) ) ;
#519 = CARTESIAN_POINT ( 'NONE',  ( 0.000000000000000000, 0.000000000000000000, 0.000000000000000000 ) ) ;
#520 = AXIS2_PLACEMENT_3D ( 'NONE', #3033, #5131, #3456 ) ;
#521 = DIRECTION ( 'NONE',  ( 1.000000000000000000, 0.000000000000000000, 0.000000000000000000 ) ) ;
#522 = LINE ( 'NONE', #2878, #4544 ) ;
#523 = CARTESIAN_POINT ( 'NONE',  ( 0.000000000000000000, 0.000000000000000000, 8.000000000000000000 ) ) ;
#524 = PLANE ( 'NONE',  #1617 ) ;
#525 = VERTEX_POINT ( 'NONE', #4460 ) ;
#526 = DIRECTION ( 'NONE',  ( 1.000000000000000000, 0.000000000000000000, 0.000000000000000000 ) ) ;
#527 = CARTESIAN_POINT ( 'NONE',  ( -8.765969750978372943, 5.050798838973364902, 14.00000000000000000 ) ) ;
#528 = CARTESIAN_POINT ( 'NONE',  ( -0.8890388043606449742, 7.706404363472288743, 1.999999999999998224 ) ) ;
#529 = VECTOR ( 'NONE', #2822, 1000.000000000000000 ) ;
#530 = EDGE_CURVE ( 'NONE', #964, #1719, #3971, .T. ) ;
#531 = CARTESIAN_POINT ( 'NONE',  ( -5.048038583874033591, -7.300734008993713609, 1.999999999999998224 ) ) ;
#532 = CARTESIAN_POINT ( 'NONE',  ( -6.398096652174581678, -7.548242073784473760, 14.00000000000000000 ) ) ;
#533 = VECTOR ( 'NONE', #2608, 1000.000000000000000 ) ;
#534 = VERTEX_POINT ( 'NONE', #2654 ) ;
#535 = CARTESIAN_POINT ( 'NONE',  ( -3.287100391418392942, 10.22059872437900019, 1.999999999999998224 ) ) ;
#536 = CARTESIAN_POINT ( 'NONE',  ( 3.896371052708265559, -4.167854722423870228, 14.00000000000000000 ) ) ;
#537 = CARTESIAN_POINT ( 'NONE',  ( -5.210352092881700869, -6.569156856910654874, 13.99999999999999645 ) ) ;
#538 = CARTESIAN_POINT ( 'NONE',  ( 3.747087600548785868, -7.295897990121166465, 13.99999999999999645 ) ) ;
#539 = CARTESIAN_POINT ( 'NONE',  ( -6.069783318623454882, -0.2142533344233820691, 14.00000000000000000 ) ) ;
#540 = CARTESIAN_POINT ( 'NONE',  ( -2.153669193480073574, -8.035861145135083206, 1.999999999999998224 ) ) ;
#541 = CARTESIAN_POINT ( 'NONE',  ( 4.999999999999914735, 24.49489742783179835, -8.000000000000000000 ) ) ;
#542 = DIRECTION ( 'NONE',  ( -1.000000000000000000, 0.000000000000000000, 0.000000000000000000 ) ) ;
#543 = LINE ( 'NONE', #4401, #4361 ) ;
#544 = ORIENTED_EDGE ( 'NONE', *, *, #3049, .T. ) ;
#545 = DIRECTION ( 'NONE',  ( -0.000000000000000000, -0.000000000000000000, 1.000000000000000000 ) ) ;
#546 = CARTESIAN_POINT ( 'NONE',  ( -5.399999999999998579, 26.45448922205832787, 12.00000000000000000 ) ) ;
#547 = CARTESIAN_POINT ( 'NONE',  ( 0.000000000000000000, 0.000000000000000000, -8.000000000000000000 ) ) ;
#548 = CARTESIAN_POINT ( 'NONE',  ( -5.651290410005071152, 9.082320918485368821, 13.99999999999999645 ) ) ;
#549 = SURFACE_STYLE_USAGE ( .BOTH. , #2796 ) ;
#550 = CARTESIAN_POINT ( 'NONE',  ( 6.000000000000000000, 0.000000000000000000, 1.999999999999998224 ) ) ;
#551 = ORIENTED_EDGE ( 'NONE', *, *, #167, .T. ) ;
#552 = ORIENTED_EDGE ( 'NONE', *, *, #1022, .F. ) ;
#553 = CARTESIAN_POINT ( 'NONE',  ( -5.592500163774714039, 7.275211197852027745, 14.00000000000000000 ) ) ;
#554 = CARTESIAN_POINT ( 'NONE',  ( 7.025143070632193343, -0.1151745751371896220, 1.999999999999998224 ) ) ;
#555 = CARTESIAN_POINT ( 'NONE',  ( -9.031632682309719939, 0.1436733667526190195, 1.999999999999998224 ) ) ;
#556 = CARTESIAN_POINT ( 'NONE',  ( -2.067895747887562141, -9.596367745172036834, 14.00000000000000000 ) ) ;
#557 = ORIENTED_EDGE ( 'NONE', *, *, #149, .F. ) ;
#558 = CARTESIAN_POINT ( 'NONE',  ( -7.035243215357268376, 8.023489478516459883, 1.999999999999998224 ) ) ;
#559 = EDGE_CURVE ( 'NONE', #5009, #2746, #334, .T. ) ;
#560 = CARTESIAN_POINT ( 'NONE',  ( 5.500000000000001776, 0.000000000000000000, 14.00000000000000000 ) ) ;
#561 = CARTESIAN_POINT ( 'NONE',  ( 0.5432484998931954578, -8.249156888542636068, 13.99999999999999645 ) ) ;
#562 = CARTESIAN_POINT ( 'NONE',  ( 5.526041665711820983, -0.8982374663919268087, 14.00000000000000000 ) ) ;
#563 = ORIENTED_EDGE ( 'NONE', *, *, #3394, .F. ) ;
#564 = CARTESIAN_POINT ( 'NONE',  ( -8.026550172065139321, -2.724140490265046122, 1.999999999999998224 ) ) ;
#565 = FACE_OUTER_BOUND ( 'NONE', #5136, .T. ) ;
#566 = CARTESIAN_POINT ( 'NONE',  ( 2.161943361801394570, -6.363123982928429179, 1.999999999999998224 ) ) ;
#567 = ORIENTED_EDGE ( 'NONE', *, *, #695, .F. ) ;
#568 = CARTESIAN_POINT ( 'NONE',  ( 4.848934754808810865, -4.539135254905419359, 1.999999999999998224 ) ) ;
#569 = CARTESIAN_POINT ( 'NONE',  ( 4.999999999999914735, 24.49489742783179835, 8.000000000000000000 ) ) ;
#570 = EDGE_CURVE ( 'NONE', #3843, #2002, #3145, .T. ) ;
#571 = CARTESIAN_POINT ( 'NONE',  ( -6.576488680450180979, -0.2289623203888878078, 13.99999999999999645 ) ) ;
#572 = ADVANCED_FACE ( 'NONE', ( #4032 ), #4002, .T. ) ;
#573 = AXIS2_PLACEMENT_3D ( 'NONE', #5087, #2065, #1144 ) ;
#574 = CARTESIAN_POINT ( 'NONE',  ( 0.000000000000000000, 0.000000000000000000, 12.00000000000000000 ) ) ;
#575 = UNCERTAINTY_MEASURE_WITH_UNIT (LENGTH_MEASURE( 1.000000000000000082E-05 ), #4830, 'distance_accuracy_value', 'NONE');
#576 = LINE ( 'NONE', #638, #774 ) ;
#577 = LINE ( 'NONE', #4896, #1520 ) ;
#578 = ORIENTED_EDGE ( 'NONE', *, *, #2981, .F. ) ;
#579 = LINE ( 'NONE', #2332, #2349 ) ;
#580 = CARTESIAN_POINT ( 'NONE',  ( -9.031632682309723492, 0.1436733667526614300, 14.00000000000000000 ) ) ;
#581 = CARTESIAN_POINT ( 'NONE',  ( -6.465640026559585252, 4.020973141381892546, 1.999999999999998224 ) ) ;
#582 = AXIS2_PLACEMENT_3D ( 'NONE', #3488, #2656, #3891 ) ;
#583 = CARTESIAN_POINT ( 'NONE',  ( 7.925371078819430259, 2.990572132494937474, 1.999999999999998224 ) ) ;
#584 = CARTESIAN_POINT ( 'NONE',  ( -8.757712506721391676, -2.046213373001789737, 14.00000000000000000 ) ) ;
#585 = EDGE_CURVE ( 'NONE', #2034, #5308, #1351, .T. ) ;
#586 = VERTEX_POINT ( 'NONE', #461 ) ;
#587 = CARTESIAN_POINT ( 'NONE',  ( 11.00000000000000355, -2.485533480423018915E-14, 1.999999999999998224 ) ) ;
#588 = AXIS2_PLACEMENT_3D ( 'NONE', #5265, #4773, #1322 ) ;
#589 = CARTESIAN_POINT ( 'NONE',  ( -5.525185448606695360, 2.707100724334913444, 14.00000000000000000 ) ) ;
#590 = CARTESIAN_POINT ( 'NONE',  ( 8.454926800553035804, -3.338224220245739726, 13.99999999999999645 ) ) ;
#591 = VECTOR ( 'NONE', #721, 999.9999999999998863 ) ;
#592 = CARTESIAN_POINT ( 'NONE',  ( -5.748891254250207083, -8.037420881456807109, 1.999999999999998224 ) ) ;
#593 = EDGE_LOOP ( 'NONE', ( #4807, #5299, #2400, #5252 ) ) ;
#594 = CARTESIAN_POINT ( 'NONE',  ( 8.396466517619506575, 3.163083589105210258, 1.999999999999998224 ) ) ;
#595 = AXIS2_PLACEMENT_3D ( 'NONE', #235, #4212, #754 ) ;
#596 = APPLICATION_CONTEXT ( 'automotive_design' ) ;
#597 = CARTESIAN_POINT ( 'NONE',  ( 1.300000000000000044, 0.000000000000000000, 0.000000000000000000 ) ) ;
#598 = EDGE_CURVE ( 'NONE', #4504, #73, #1734, .T. ) ;
#599 = SURFACE_STYLE_USAGE ( .BOTH. , #3222 ) ;
#600 = CARTESIAN_POINT ( 'NONE',  ( -1.105557477332586247, -6.708264047591375956, 1.999999999999998224 ) ) ;
#601 = AXIS2_PLACEMENT_3D ( 'NONE', #4698, #1222, #441 ) ;
#602 = ORIENTED_EDGE ( 'NONE', *, *, #3162, .F. ) ;
#603 = CARTESIAN_POINT ( 'NONE',  ( -2.189112655477410740, -6.464091385745793339, 1.999999999999998224 ) ) ;
#604 = DIRECTION ( 'NONE',  ( -1.000000000000000000, -0.000000000000000000, -0.000000000000000000 ) ) ;
#605 =( NAMED_UNIT ( * ) SI_UNIT ( $, .STERADIAN. ) SOLID_ANGLE_UNIT ( ) );
#606 = CIRCLE ( 'NONE', #4005, 22.00000000000000000 ) ;
#607 = AXIS2_PLACEMENT_3D ( 'NONE', #2707, #486, #5329 ) ;
#608 = LINE ( 'NONE', #5502, #3645 ) ;
#609 = ORIENTED_EDGE ( 'NONE', *, *, #5454, .T. ) ;
#610 = DIRECTION ( 'NONE',  ( -1.000000000000000000, 0.000000000000000000, 0.000000000000000000 ) ) ;
#611 = CARTESIAN_POINT ( 'NONE',  ( -0.7616497023963333390, 9.236585841461440793, 14.00000000000000000 ) ) ;
#612 = VECTOR ( 'NONE', #526, 1000.000000000000000 ) ;
#613 = CARTESIAN_POINT ( 'NONE',  ( -5.390757458300977412, 6.793134358447004750, 1.999999999999998224 ) ) ;
#614 = VECTOR ( 'NONE', #4305, 1000.000000000000000 ) ;
#615 = CARTESIAN_POINT ( 'NONE',  ( -7.986673696634112751, -0.6581801297105769333, 1.999999999999998224 ) ) ;
#616 = CARTESIAN_POINT ( 'NONE',  ( 8.549805251451807919, -4.382211019330642721, 14.00000000000000000 ) ) ;
#617 = CARTESIAN_POINT ( 'NONE',  ( 0.000000000000000000, 0.000000000000000000, -2.000000000000000000 ) ) ;
#618 = ORIENTED_EDGE ( 'NONE', *, *, #1353, .F. ) ;
#619 = AXIS2_PLACEMENT_3D ( 'NONE', #3226, #1030, #1523 ) ;
#620 = PLANE ( 'NONE',  #2643 ) ;
#621 = CARTESIAN_POINT ( 'NONE',  ( -5.021280548128706833, 3.603657539914777885, 14.00000000000094147 ) ) ;
#622 = ADVANCED_BREP_SHAPE_REPRESENTATION ( '', ( #698, #1336 ), #5443 ) ;
#623 = CARTESIAN_POINT ( 'NONE',  ( 0.3355163285737458034, -10.27362971114551371, 13.99999999999999645 ) ) ;
#624 = EDGE_CURVE ( 'NONE', #2461, #2258, #1720, .T. ) ;
#625 = AXIS2_PLACEMENT_3D ( 'NONE', #1558, #3738, #1899 ) ;
#626 = CARTESIAN_POINT ( 'NONE',  ( 2.667884741302309237, 9.975564253400264647, 1.999999999999998224 ) ) ;
#627 = ORIENTED_EDGE ( 'NONE', *, *, #328, .T. ) ;
#628 = CARTESIAN_POINT ( 'NONE',  ( 4.683456943470878819, 7.530568860026273015, 1.999999999999998224 ) ) ;
#629 = LINE ( 'NONE', #194, #3082 ) ;
#630 = SURFACE_STYLE_FILL_AREA ( #1056 ) ;
#631 = CARTESIAN_POINT ( 'NONE',  ( 6.160418207306092242, 1.983851483784910164, 1.999999999999998224 ) ) ;
#632 = ORIENTED_EDGE ( 'NONE', *, *, #3010, .T. ) ;
#633 = CARTESIAN_POINT ( 'NONE',  ( 1.540339863274624577, 7.144097608501353669, 1.999999999999998224 ) ) ;
#634 = DIRECTION ( 'NONE',  ( 0.000000000000000000, -0.8660254037844385966, 0.5000000000000001110 ) ) ;
#635 = CARTESIAN_POINT ( 'NONE',  ( 1.623707939105870413, -6.078451570951948213, 13.99999999999999645 ) ) ;
#636 = PRODUCT_DEFINITION_SHAPE ( 'NONE', 'NONE',  #5693 ) ;
#637 = FACE_OUTER_BOUND ( 'NONE', #4150, .T. ) ;
#638 = CARTESIAN_POINT ( 'NONE',  ( 23.48484848484848442, -8.570991287109677614, 8.000000000000000000 ) ) ;
#639 = DIRECTION ( 'NONE',  ( 0.000000000000000000, 0.000000000000000000, -1.000000000000000000 ) ) ;
#640 = ORIENTED_EDGE ( 'NONE', *, *, #4759, .T. ) ;
#641 = LINE ( 'NONE', #3712, #1066 ) ;
#642 = CARTESIAN_POINT ( 'NONE',  ( 10.36702220812670028, 1.720931399333114120, 14.00000000000000000 ) ) ;
#643 = CARTESIAN_POINT ( 'NONE',  ( 8.164254108709977586, -4.026826083952141033, 1.999999999999998224 ) ) ;
#644 = CARTESIAN_POINT ( 'NONE',  ( -7.763712483375483586, -3.368527140561099031, 13.99999999999999645 ) ) ;
#645 = CARTESIAN_POINT ( 'NONE',  ( -1.271096247112533995, -9.720655361064800104, 1.999999999999998224 ) ) ;
#646 = CARTESIAN_POINT ( 'NONE',  ( 9.320190601378300244, -2.164585516638619200, 14.00000000000000000 ) ) ;
#647 = DIRECTION ( 'NONE',  ( -0.000000000000000000, -0.000000000000000000, -1.000000000000000000 ) ) ;
#648 = ORIENTED_EDGE ( 'NONE', *, *, #866, .T. ) ;
#649 = CYLINDRICAL_SURFACE ( 'NONE', #3107, 1.999999999999999112 ) ;
#650 = CARTESIAN_POINT ( 'NONE',  ( 6.340368144647111848, -1.697206311171021831, 14.00000000000000000 ) ) ;
#651 = CARTESIAN_POINT ( 'NONE',  ( -9.026614039607444795, -2.903226997913483487, 13.99999999999999645 ) ) ;
#652 = MANIFOLD_SOLID_BREP ( 'Fillet1', #3277 ) ;
#653 = EDGE_CURVE ( 'NONE', #2224, #1028, #888, .T. ) ;
#654 = CARTESIAN_POINT ( 'NONE',  ( -4.668631340267960894, 9.078485505801564770, 1.999999999999998224 ) ) ;
#655 = ORIENTED_EDGE ( 'NONE', *, *, #4575, .F. ) ;
#656 = CARTESIAN_POINT ( 'NONE',  ( 7.748217264256983761, 4.472783157626249562, 1.999999999999998224 ) ) ;
#657 = DIRECTION ( 'NONE',  ( 0.000000000000000000, 0.000000000000000000, 1.000000000000000000 ) ) ;
#658 =( LENGTH_UNIT ( ) NAMED_UNIT ( * ) SI_UNIT ( .MILLI., .METRE. ) );
#659 = CARTESIAN_POINT ( 'NONE',  ( -3.597458971453999066, 6.226096630968013024, 1.999999999999998224 ) ) ;
#660 = VERTEX_POINT ( 'NONE', #4381 ) ;
#661 = CARTESIAN_POINT ( 'NONE',  ( 6.268835244667307904, -4.335177162149147279, 1.999999999999998224 ) ) ;
#662 = CARTESIAN_POINT ( 'NONE',  ( 0.000000000000000000, 0.000000000000000000, 4.000000000000000000 ) ) ;
#663 = FACE_OUTER_BOUND ( 'NONE', #2351, .T. ) ;
#664 = CARTESIAN_POINT ( 'NONE',  ( 1.300000000000000044, -1.443375672974063884, -3.691112476943992763E-18 ) ) ;
#665 = UNCERTAINTY_MEASURE_WITH_UNIT (LENGTH_MEASURE( 1.000000000000000082E-05 ), #5331, 'distance_accuracy_value', 'NONE');
#666 = DIRECTION ( 'NONE',  ( -1.000000000000000000, -0.000000000000000000, -0.000000000000000000 ) ) ;
#667 = ORIENTED_EDGE ( 'NONE', *, *, #1697, .T. ) ;
#668 = CARTESIAN_POINT ( 'NONE',  ( 2.000000000000000000, 0.000000000000000000, 8.000000000000000000 ) ) ;
#669 = FACE_OUTER_BOUND ( 'NONE', #3074, .T. ) ;
#670 = CARTESIAN_POINT ( 'NONE',  ( -1.063411474431080306, -9.238278818534249481, 1.999999999999998224 ) ) ;
#671 = CARTESIAN_POINT ( 'NONE',  ( -6.848710654519975627, 5.255840572796830479, 13.99999999999999645 ) ) ;
#672 = LINE ( 'NONE', #2886, #5086 ) ;
#673 = EDGE_LOOP ( 'NONE', ( #3634, #1342, #551, #4466 ) ) ;
#674 = LINE ( 'NONE', #4556, #1058 ) ;
#675 = ORIENTED_EDGE ( 'NONE', *, *, #3739, .T. ) ;
#676 = CARTESIAN_POINT ( 'NONE',  ( 1.300000000000000044, 0.7216878364870328300, 1.249999999999999778 ) ) ;
#677 = CARTESIAN_POINT ( 'NONE',  ( -4.975175822334874098, 5.137265612443751017, 14.00000000000000000 ) ) ;
#678 = CARTESIAN_POINT ( 'NONE',  ( -6.537688394901546296, -6.759197365499824528, 13.99999999999999645 ) ) ;
#679 = EDGE_CURVE ( 'NONE', #5392, #4001, #437, .T. ) ;
#680 = CARTESIAN_POINT ( 'NONE',  ( -6.876639332705559937, 1.598006320995821516, 14.00000000000000000 ) ) ;
#681 = AXIS2_PLACEMENT_3D ( 'NONE', #5350, #27, #3508 ) ;
#682 = EDGE_LOOP ( 'NONE', ( #5307, #2020, #1568, #4865 ) ) ;
#683 = CARTESIAN_POINT ( 'NONE',  ( -10.42442484909470046, -1.371544430045556373, 1.999999999999998224 ) ) ;
#684 = PRODUCT_DEFINITION_SHAPE ( 'NONE', 'NONE',  #4858 ) ;
#685 = CIRCLE ( 'NONE', #222, 0.2500000000000002220 ) ;
#686 = CARTESIAN_POINT ( 'NONE',  ( -4.999999999999998224, 24.49489742783178414, 12.00000000000000000 ) ) ;
#687 = EDGE_CURVE ( 'NONE', #2844, #5686, #1361, .T. ) ;
#688 = CARTESIAN_POINT ( 'NONE',  ( 4.064490656457592443, -6.524520197619557926, 1.999999999999998224 ) ) ;
#689 = ORIENTED_EDGE ( 'NONE', *, *, #1022, .T. ) ;
#690 = CARTESIAN_POINT ( 'NONE',  ( 6.496939485553420823, 0.4301729194711073623, 1.999999999999998224 ) ) ;
#691 = VECTOR ( 'NONE', #3676, 1000.000000000000000 ) ;
#692 = CARTESIAN_POINT ( 'NONE',  ( -3.886954398759499885, 5.424498719065524277, 1.999999999999998224 ) ) ;
#693 = CARTESIAN_POINT ( 'NONE',  ( 7.025143070632195119, -0.1151745751371588272, 13.99999999999999645 ) ) ;
#694 = ADVANCED_BREP_SHAPE_REPRESENTATION ( '', ( #4492, #1336 ), #3242 ) ;
#695 = EDGE_CURVE ( 'NONE', #5417, #2009, #2414, .T. ) ;
#696 = AXIS2_PLACEMENT_3D ( 'NONE', #2101, #4689, #3000 ) ;
#697 = DIRECTION ( 'NONE',  ( 1.000000000000000000, 0.000000000000000000, 0.000000000000000000 ) ) ;
#698 = MANIFOLD_SOLID_BREP ( 'Hex', #3733 ) ;
#699 = DIRECTION ( 'NONE',  ( -1.000000000000000000, -0.000000000000000000, -0.000000000000000000 ) ) ;
#700 = EDGE_LOOP ( 'NONE', ( #2599, #2976, #1076 ) ) ;
#701 = AXIS2_PLACEMENT_3D ( 'NONE', #1249, #817, #1709 ) ;
#702 = CARTESIAN_POINT ( 'NONE',  ( -22.50000000000000355, 0.000000000000000000, 14.00000000000000000 ) ) ;
#703 = CARTESIAN_POINT ( 'NONE',  ( 1.300000000000000044, -0.7216878364870318308, 1.249999999999999778 ) ) ;
#704 = CARTESIAN_POINT ( 'NONE',  ( -2.263950162103713915, 8.438937471999857109, 1.999999999999998224 ) ) ;
#705 = CARTESIAN_POINT ( 'NONE',  ( -4.372214883940321428, 6.312905667202753257, 13.99999999999999645 ) ) ;
#706 = AXIS2_PLACEMENT_3D ( 'NONE', #231, #639, #3316 ) ;
#707 = DIRECTION ( 'NONE',  ( 0.000000000000000000, 0.000000000000000000, -1.000000000000000000 ) ) ;
#708 = ORIENTED_EDGE ( 'NONE', *, *, #2114, .T. ) ;
#709 = CARTESIAN_POINT ( 'NONE',  ( 0.000000000000000000, 0.000000000000000000, 11.00000000000000000 ) ) ;
#710 = VECTOR ( 'NONE', #902, 1000.000000000000000 ) ;
#711 = ORIENTED_EDGE ( 'NONE', *, *, #4312, .T. ) ;
#712 = CARTESIAN_POINT ( 'NONE',  ( 2.400000000000000799, 0.000000000000000000, 0.000000000000000000 ) ) ;
#713 = CARTESIAN_POINT ( 'NONE',  ( 6.496939485553422600, 0.4301729194711386151, 14.00000000000000000 ) ) ;
#714 = CARTESIAN_POINT ( 'NONE',  ( 0.7976699882155482424, 9.763020831628288931, 13.99999999999999645 ) ) ;
#715 = AXIS2_PLACEMENT_3D ( 'NONE', #547, #1756, #4837 ) ;
#716 = CARTESIAN_POINT ( 'NONE',  ( 4.848934754808812642, -4.539135254905673378, 14.00000000000000000 ) ) ;
#717 = VECTOR ( 'NONE', #3845, 1000.000000000000000 ) ;
#718 = ORIENTED_EDGE ( 'NONE', *, *, #1122, .F. ) ;
#719 = CARTESIAN_POINT ( 'NONE',  ( 10.02239396097947655, -0.6576683464576721372, 1.999999999999998224 ) ) ;
#720 = AXIS2_PLACEMENT_3D ( 'NONE', #2496, #3826, #4630 ) ;
#721 = DIRECTION ( 'NONE',  ( -0.000000000000000000, -0.4999999999999999445, -0.8660254037844387076 ) ) ;
#722 = CARTESIAN_POINT ( 'NONE',  ( -1.480145937554574020, 8.115026467928048604, 1.999999999999998224 ) ) ;
#723 = CARTESIAN_POINT ( 'NONE',  ( 0.000000000000000000, 0.000000000000000000, 12.00000000000000000 ) ) ;
#724 = CARTESIAN_POINT ( 'NONE',  ( 4.366464973618273682, -5.686602709308030690, 13.99999999999999645 ) ) ;
#725 = DIRECTION ( 'NONE',  ( -0.000000000000000000, -0.000000000000000000, 1.000000000000000000 ) ) ;
#726 = VERTEX_POINT ( 'NONE', #4122 ) ;
#727 = DIRECTION ( 'NONE',  ( 0.000000000000000000, 0.000000000000000000, -1.000000000000000000 ) ) ;
#728 = DIRECTION ( 'NONE',  ( 1.000000000000000000, 0.000000000000000000, 0.000000000000000000 ) ) ;
#729 = CARTESIAN_POINT ( 'NONE',  ( -0.1462562576243746360, 8.775315755191545719, 1.999999999999998224 ) ) ;
#730 = CARTESIAN_POINT ( 'NONE',  ( 7.422282976138728117, -5.315384720684047437, 13.99999999999999645 ) ) ;
#731 = CARTESIAN_POINT ( 'NONE',  ( 5.000000000000001776, 24.49489742783178414, 4.000000000000000000 ) ) ;
#732 = ORIENTED_EDGE ( 'NONE', *, *, #5425, .T. ) ;
#733 = DIRECTION ( 'NONE',  ( -1.000000000000000000, 0.000000000000000000, 0.000000000000000000 ) ) ;
#734 = ORIENTED_EDGE ( 'NONE', *, *, #788, .F. ) ;
#735 = CARTESIAN_POINT ( 'NONE',  ( 0.000000000000000000, 1.443375672974065216, 7.017607234860990640E-28 ) ) ;
#736 = CARTESIAN_POINT ( 'NONE',  ( 3.621982275015807939, -5.614208739972780471, 14.00000000000000000 ) ) ;
#737 = CARTESIAN_POINT ( 'NONE',  ( -1.063411474431080528, -9.238278818535565762, 13.99999999999999645 ) ) ;
#738 = CARTESIAN_POINT ( 'NONE',  ( -4.184906021401652687, -5.457255036755483069, 14.00000000000000000 ) ) ;
#739 = ORIENTED_EDGE ( 'NONE', *, *, #1001, .T. ) ;
#740 = CARTESIAN_POINT ( 'NONE',  ( 5.800093669797941054, -8.375184749302256648, 1.999999999999998224 ) ) ;
#741 = CARTESIAN_POINT ( 'NONE',  ( 0.000000000000000000, -1.443375672974063884, -3.691112476943992763E-18 ) ) ;
#742 =( NAMED_UNIT ( * ) PLANE_ANGLE_UNIT ( ) SI_UNIT ( $, .RADIAN. ) );
#743 = CARTESIAN_POINT ( 'NONE',  ( 3.810368753942602993, 7.433568398487427231, 1.999999999999998224 ) ) ;
#744 = DIRECTION ( 'NONE',  ( -1.000000000000000000, 0.000000000000000000, 0.000000000000000000 ) ) ;
#745 = CARTESIAN_POINT ( 'NONE',  ( -2.352725117874390648, -6.938351456669185069, 13.99999999999999645 ) ) ;
#746 = FILL_AREA_STYLE ('',( #1584 ) ) ;
#747 = CARTESIAN_POINT ( 'NONE',  ( -7.304208470130000741, 7.056621303511527721, 1.999999999999998224 ) ) ;
#748 = EDGE_CURVE ( 'NONE', #4516, #5521, #2767, .T. ) ;
#749 = DIRECTION ( 'NONE',  ( -1.000000000000000000, 0.000000000000000000, -0.000000000000000000 ) ) ;
#750 = FACE_OUTER_BOUND ( 'NONE', #5246, .T. ) ;
#751 = ORIENTED_EDGE ( 'NONE', *, *, #1982, .T. ) ;
#752 = EDGE_CURVE ( 'NONE', #5339, #4697, #142, .T. ) ;
#753 = FACE_OUTER_BOUND ( 'NONE', #4274, .T. ) ;
#754 = DIRECTION ( 'NONE',  ( 1.000000000000000000, 0.000000000000000000, 0.000000000000000000 ) ) ;
#755 = CARTESIAN_POINT ( 'NONE',  ( 8.454926800553035804, -3.338224220245739726, 13.99999999999999645 ) ) ;
#756 = CARTESIAN_POINT ( 'NONE',  ( 25.00000000000000000, 3.061616997868383043E-15, 0.000000000000000000 ) ) ;
#757 = EDGE_LOOP ( 'NONE', ( #4197, #5327, #4355, #3268, #3669, #1822, #2688 ) ) ;
#758 = CARTESIAN_POINT ( 'NONE',  ( 5.000000000000001776, 24.49489742783178414, 12.00000000000000000 ) ) ;
#759 = COLOUR_RGB ( '',0.8941176470588234615, 0.8941176470588234615, 0.8941176470588234615 ) ;
#760 = VERTEX_POINT ( 'NONE', #4973 ) ;
#761 = LINE ( 'NONE', #5191, #3103 ) ;
#762 = CARTESIAN_POINT ( 'NONE',  ( -0.5497243705170608008, -6.763214047005219776, 14.00000000000000000 ) ) ;
#763 = CARTESIAN_POINT ( 'NONE',  ( -6.726831604608805470, -7.927219868181097695, 13.99999999999999645 ) ) ;
#764 = ADVANCED_FACE ( 'NONE', ( #112 ), #4631, .F. ) ;
#765 = CARTESIAN_POINT ( 'NONE',  ( 2.227988792049260702, 5.923272706910787555, 14.00000000000000000 ) ) ;
#766 = ORIENTED_EDGE ( 'NONE', *, *, #23, .T. ) ;
#767 = CARTESIAN_POINT ( 'NONE',  ( -1.342170334697201595, -10.21728332006300199, 1.999999999999998224 ) ) ;
#768 = CYLINDRICAL_SURFACE ( 'NONE', #3356, 25.00000000000000000 ) ;
#769 = AXIS2_PLACEMENT_3D ( 'NONE', #4923, #2711, #4495 ) ;
#770 = DIRECTION ( 'NONE',  ( 0.000000000000000000, 0.000000000000000000, -1.000000000000000000 ) ) ;
#771 = CARTESIAN_POINT ( 'NONE',  ( -3.987536574860945038, 7.161134007378406885, 1.999999999999998224 ) ) ;
#772 = LINE ( 'NONE', #281, #3560 ) ;
#773 = CARTESIAN_POINT ( 'NONE',  ( -4.310533329765174670, 5.077046166955135220, 13.99999999999952927 ) ) ;
#774 = VECTOR ( 'NONE', #2388, 1000.000000000000000 ) ;
#775 = ADVANCED_FACE ( 'NONE', ( #4519, #5412 ), #2791, .T. ) ;
#776 = CARTESIAN_POINT ( 'NONE',  ( 2.992331685656917539, 8.840389773664522721, 1.999999999999998224 ) ) ;
#777 = AXIS2_PLACEMENT_3D ( 'NONE', #4406, #5273, #4868 ) ;
#778 = DIRECTION ( 'NONE',  ( 0.000000000000000000, 0.000000000000000000, 1.000000000000000000 ) ) ;
#779 = LINE ( 'NONE', #2042, #2167 ) ;
#780 = ORIENTED_EDGE ( 'NONE', *, *, #5104, .F. ) ;
#781 = DIRECTION ( 'NONE',  ( 1.000000000000000000, 0.000000000000000000, 0.000000000000000000 ) ) ;
#782 = DIRECTION ( 'NONE',  ( 0.000000000000000000, 0.000000000000000000, -1.000000000000000000 ) ) ;
#783 = CARTESIAN_POINT ( 'NONE',  ( -9.533152408061619454, 0.1566715252476607312, 13.99999999999999645 ) ) ;
#784 = DIRECTION ( 'NONE',  ( -1.000000000000000000, 0.000000000000000000, -0.000000000000000000 ) ) ;
#786 = ORIENTED_EDGE ( 'NONE', *, *, #5454, .F. ) ;
#785 = AXIS2_PLACEMENT_3D ( 'NONE', #3064, #2598, #871 ) ;
#787 = FACE_OUTER_BOUND ( 'NONE', #1791, .T. ) ;
#788 = EDGE_CURVE ( 'NONE', #1305, #1719, #3740, .T. ) ;
#789 = ORIENTED_EDGE ( 'NONE', *, *, #2529, .F. ) ;
#790 = DIRECTION ( 'NONE',  ( -1.000000000000000000, 0.000000000000000000, 0.000000000000000000 ) ) ;
#791 = CARTESIAN_POINT ( 'NONE',  ( -0.1241967792452473573, -7.777596356722547455, 14.00000000000000000 ) ) ;
#792 = CARTESIAN_POINT ( 'NONE',  ( -0.8811140424828312057, 6.693995663234410642, 1.999999999999998224 ) ) ;
#793 = PRODUCT_DEFINITION_CONTEXT ( 'detailed design', #822, 'design' ) ;
#794 = VECTOR ( 'NONE', #5528, 1000.000000000000000 ) ;
#795 = DIRECTION ( 'NONE',  ( 0.000000000000000000, 0.000000000000000000, 1.000000000000000000 ) ) ;
#796 = CARTESIAN_POINT ( 'NONE',  ( -6.742266116715659230, -1.811900715328871092, 14.00000000000000000 ) ) ;
#797 = ORIENTED_EDGE ( 'NONE', *, *, #598, .T. ) ;
#798 = VECTOR ( 'NONE', #1497, 1000.000000000000114 ) ;
#799 = CARTESIAN_POINT ( 'NONE',  ( -3.290073422422500560, -8.739709727800574868, 1.999999999999998224 ) ) ;
#800 = EDGE_CURVE ( 'NONE', #3462, #2713, #891, .T. ) ;
#801 = DIRECTION ( 'NONE',  ( -1.000000000000000000, 0.000000000000000000, 0.000000000000000000 ) ) ;
#802 = AXIS2_PLACEMENT_3D ( 'NONE', #5681, #2572, #3811 ) ;
#803 = CARTESIAN_POINT ( 'NONE',  ( 8.477027301005913174, -1.108685663976167080, 1.999999999999998224 ) ) ;
#804 = CARTESIAN_POINT ( 'NONE',  ( 0.000000000000000000, 0.000000000000000000, -8.000000000000000000 ) ) ;
#805 = AXIS2_PLACEMENT_3D ( 'NONE', #2161, #2766, #5035 ) ;
#806 = CARTESIAN_POINT ( 'NONE',  ( 0.5931392160223177834, -7.236979168992432321, 13.99999999999999645 ) ) ;
#807 = CARTESIAN_POINT ( 'NONE',  ( 9.348788865897812883, 1.705571004836294646, 1.999999999999998224 ) ) ;
#808 = VECTOR ( 'NONE', #3588, 1000.000000000000000 ) ;
#809 = CARTESIAN_POINT ( 'NONE',  ( 21.75000000000000000, -3.307189138830739061, -58.22539674441618018 ) ) ;
#810 = DIRECTION ( 'NONE',  ( -0.000000000000000000, -0.000000000000000000, 1.000000000000000000 ) ) ;
#811 = ORIENTED_EDGE ( 'NONE', *, *, #5425, .F. ) ;
#812 = CARTESIAN_POINT ( 'NONE',  ( 21.99999999999999645, -30.00000000000000000, 4.000000000000001776 ) ) ;
#813 = DIRECTION ( 'NONE',  ( -1.000000000000000000, -0.000000000000000000, -0.000000000000000000 ) ) ;
#814 = CARTESIAN_POINT ( 'NONE',  ( -8.402144917908875854, 4.670158400850172420, 13.99999999999999645 ) ) ;
#815 = DIRECTION ( 'NONE',  ( 1.000000000000000000, 0.000000000000000000, 0.000000000000000000 ) ) ;
#816 = ORIENTED_EDGE ( 'NONE', *, *, #4686, .T. ) ;
#817 = DIRECTION ( 'NONE',  ( 0.000000000000000000, 0.000000000000000000, -1.000000000000000000 ) ) ;
#818 = ORIENTED_EDGE ( 'NONE', *, *, #1286, .T. ) ;
#819 = LINE ( 'NONE', #5620, #3283 ) ;
#820 = CARTESIAN_POINT ( 'NONE',  ( 6.591354251721611490, -5.587324598951901145, 14.00000000000000000 ) ) ;
#821 = CARTESIAN_POINT ( 'NONE',  ( -6.112420884766618379, -2.295018720694776526, 1.999999999999998224 ) ) ;
#822 = APPLICATION_CONTEXT ( 'automotive_design' ) ;
#823 = CARTESIAN_POINT ( 'NONE',  ( 0.000000000000000000, -1.443375672974063884, -3.691112476943992763E-18 ) ) ;
#824 = CARTESIAN_POINT ( 'NONE',  ( -6.281085993838468440, -4.827840781183066809, 14.00000000000000000 ) ) ;
#825 = ADVANCED_FACE ( 'NONE', ( #663 ), #4177, .F. ) ;
#826 = ORIENTED_EDGE ( 'NONE', *, *, #5662, .F. ) ;
#827 = CARTESIAN_POINT ( 'NONE',  ( -7.035243215357268376, 8.023489478516459883, 1.999999999999998224 ) ) ;
#828 = CARTESIAN_POINT ( 'NONE',  ( -4.492165532403490147, -5.853844512260857336, 13.99999999999999645 ) ) ;
#829 = SHAPE_DEFINITION_REPRESENTATION ( #2987, #1911 ) ;
#830 = CARTESIAN_POINT ( 'NONE',  ( -2.970508497641843881, 8.737606122598624125, 1.999999999999998224 ) ) ;
#831 = CARTESIAN_POINT ( 'NONE',  ( 4.585040342817966241, 6.402697129001492904, 1.999999999999998224 ) ) ;
#832 = CARTESIAN_POINT ( 'NONE',  ( 7.748217264258252968, 4.472783157626409434, 13.99999999999999645 ) ) ;
#833 = DIRECTION ( 'NONE',  ( 0.000000000000000000, 0.000000000000000000, -1.000000000000000000 ) ) ;
#834 =( NAMED_UNIT ( * ) SI_UNIT ( $, .STERADIAN. ) SOLID_ANGLE_UNIT ( ) );
#835 = CARTESIAN_POINT ( 'NONE',  ( 8.549805251451806143, -4.382211019330641832, 1.999999999999998224 ) ) ;
#836 = CARTESIAN_POINT ( 'NONE',  ( 23.00000000000000000, -2.168404344971008868E-16, -4.000000000000000000 ) ) ;
#837 = ORIENTED_EDGE ( 'NONE', *, *, #4585, .F. ) ;
#838 = DIRECTION ( 'NONE',  ( -1.000000000000000000, -0.000000000000000000, -0.000000000000000000 ) ) ;
#839 = CARTESIAN_POINT ( 'NONE',  ( 1.999247522871012483, 8.586038698135613600, 13.99999999999999645 ) ) ;
#840 = LINE ( 'NONE', #2596, #1777 ) ;
#841 = VERTEX_POINT ( 'NONE', #4160 ) ;
#842 = DIRECTION ( 'NONE',  ( 0.000000000000000000, 0.000000000000000000, -1.000000000000000000 ) ) ;
#843 = ORIENTED_EDGE ( 'NONE', *, *, #1114, .T. ) ;
#844 = FACE_OUTER_BOUND ( 'NONE', #5680, .T. ) ;
#845 = CARTESIAN_POINT ( 'NONE',  ( -3.813875884798381577, -6.869235835554827752, 14.00000000000000000 ) ) ;
#846 = CARTESIAN_POINT ( 'NONE',  ( -5.978927507574433697, 2.933119789328457294, 1.999999999999998224 ) ) ;
#847 = DIRECTION ( 'NONE',  ( -1.000000000000000000, 0.000000000000000000, -0.000000000000000000 ) ) ;
#848 = MECHANICAL_DESIGN_GEOMETRIC_PRESENTATION_REPRESENTATION (  '', ( #4251 ), #2780 ) ;
#849 = CARTESIAN_POINT ( 'NONE',  ( 8.477027301005275461, -1.108685663976147318, 14.00000000000000000 ) ) ;
#850 = ADVANCED_FACE ( 'NONE', ( #3269 ), #1545, .T. ) ;
#851 = EDGE_LOOP ( 'NONE', ( #294, #2776 ) ) ;
#852 = CARTESIAN_POINT ( 'NONE',  ( 11.00000000000000355, -2.485533480423018915E-14, 1.999999999999998224 ) ) ;
#853 = ADVANCED_FACE ( 'NONE', ( #242 ), #4133, .T. ) ;
#854 = CARTESIAN_POINT ( 'NONE',  ( -3.886954398759500773, 5.424498719065526053, 13.99999999999999645 ) ) ;
#855 = PRODUCT_CONTEXT ( 'NONE', #5414, 'mechanical' ) ;
#856 = CARTESIAN_POINT ( 'NONE',  ( 9.164356920907600568, 2.464151434936005192, 1.999999999999998224 ) ) ;
#857 = CARTESIAN_POINT ( 'NONE',  ( -3.989331152809321157, -6.191695749071041810, 1.999999999999998224 ) ) ;
#858 = CARTESIAN_POINT ( 'NONE',  ( 6.444084565535373343, 4.617298776321548281, 13.99999999999999645 ) ) ;
#859 = CIRCLE ( 'NONE', #4991, 12.50000000000000000 ) ;
#860 = CARTESIAN_POINT ( 'NONE',  ( 23.00000000000000000, -2.168404344971008868E-16, -8.000000000000000000 ) ) ;
#861 = LINE ( 'NONE', #5267, #1138 ) ;
#862 = CARTESIAN_POINT ( 'NONE',  ( 2.149999999999998579, 0.000000000000000000, 0.000000000000000000 ) ) ;
#863 = CIRCLE ( 'NONE', #5184, 22.50000000000000355 ) ;
#864 = DIRECTION ( 'NONE',  ( 1.000000000000000000, 0.000000000000000000, 0.000000000000000000 ) ) ;
#865 = ORIENTED_EDGE ( 'NONE', *, *, #2172, .F. ) ;
#866 = EDGE_CURVE ( 'NONE', #1059, #4467, #5111, .T. ) ;
#867 = AXIS2_PLACEMENT_3D ( 'NONE', #4433, #2247, #5330 ) ;
#868 = CARTESIAN_POINT ( 'NONE',  ( 0.3355163285737458034, -10.27362971114551371, 13.99999999999999645 ) ) ;
#869 = DIRECTION ( 'NONE',  ( -3.540989467475305966E-16, -1.000000000000000000, -0.000000000000000000 ) ) ;
#870 = EDGE_LOOP ( 'NONE', ( #1828, #5276, #4459, #4079 ) ) ;
#871 = DIRECTION ( 'NONE',  ( -1.000000000000000000, 0.000000000000000000, 0.000000000000000000 ) ) ;
#872 = ORIENTED_EDGE ( 'NONE', *, *, #3851, .T. ) ;
#873 = CIRCLE ( 'NONE', #595, 25.00000000000000000 ) ;
#874 = ORIENTED_EDGE ( 'NONE', *, *, #4766, .F. ) ;
#875 = CARTESIAN_POINT ( 'NONE',  ( -7.588772809867895930, -4.728083520431684228, 14.00000000000000000 ) ) ;
#876 = CARTESIAN_POINT ( 'NONE',  ( -8.483256258862985177, -6.077987531410205868, 13.99999999999999645 ) ) ;
#877 = VECTOR ( 'NONE', #4386, 1000.000000000000000 ) ;
#878 = FACE_OUTER_BOUND ( 'NONE', #5457, .T. ) ;
#879 = CARTESIAN_POINT ( 'NONE',  ( 6.268835244667308793, -4.335177162149436825, 14.00000000000000000 ) ) ;
#880 = ORIENTED_EDGE ( 'NONE', *, *, #4681, .T. ) ;
#881 = CARTESIAN_POINT ( 'NONE',  ( -22.50000000000000355, 0.000000000000000000, 2.000000000000000000 ) ) ;
#882 = AXIS2_PLACEMENT_3D ( 'NONE', #2501, #810, #3833 ) ;
#883 = CARTESIAN_POINT ( 'NONE',  ( 1.623707939105870413, -6.078451570951948213, 13.99999999999999645 ) ) ;
#884 = SHAPE_DEFINITION_REPRESENTATION ( #3763, #143 ) ;
#885 = CARTESIAN_POINT ( 'NONE',  ( -7.966005157978614193, 4.422220743486963812, 1.999999999999998224 ) ) ;
#886 = AXIS2_PLACEMENT_3D ( 'NONE', #464, #4037, #4065 ) ;
#887 = CARTESIAN_POINT ( 'NONE',  ( -7.521311085815506559, -0.1255077825093695587, 1.999999999999998224 ) ) ;
#888 = CIRCLE ( 'NONE', #3930, 4.500000000000000000 ) ;
#889 = DIRECTION ( 'NONE',  ( -3.540989467475305966E-16, -1.000000000000000000, -0.000000000000000000 ) ) ;
#890 = FILL_AREA_STYLE ('',( #2215 ) ) ;
#891 = CIRCLE ( 'NONE', #1633, 3.799999999999999378 ) ;
#892 = CARTESIAN_POINT ( 'NONE',  ( 1.730265954310492127, 6.073542049876722970, 1.999999999999998224 ) ) ;
#893 = CARTESIAN_POINT ( 'NONE',  ( -23.00000000000000000, 0.000000000000000000, -8.000000000000000000 ) ) ;
#894 = APPLICATION_CONTEXT ( 'automotive_design' ) ;
#895 = ORIENTED_EDGE ( 'NONE', *, *, #570, .T. ) ;
#896 = DIRECTION ( 'NONE',  ( -4.364351673553916694E-15, 1.000000000000000000, 0.000000000000000000 ) ) ;
#897 = CIRCLE ( 'NONE', #250, 0.2500000000000002220 ) ;
#898 = CARTESIAN_POINT ( 'NONE',  ( 6.769338797470518365, 8.534199679355843671, 13.99999999999999645 ) ) ;
#899 = VERTEX_POINT ( 'NONE', #2864 ) ;
#900 = DIRECTION ( 'NONE',  ( -1.000000000000000000, 0.000000000000000000, 0.000000000000000000 ) ) ;
#901 = ORIENTED_EDGE ( 'NONE', *, *, #5146, .T. ) ;
#902 = DIRECTION ( 'NONE',  ( -0.000000000000000000, -0.000000000000000000, -1.000000000000000000 ) ) ;
#903 = CARTESIAN_POINT ( 'NONE',  ( -1.480145937554535385, 8.115026467927430431, 14.00000000000000000 ) ) ;
#904 = CARTESIAN_POINT ( 'NONE',  ( -3.845892476879857025, 6.661954734853423155, 1.999999999999998224 ) ) ;
#905 = CARTESIAN_POINT ( 'NONE',  ( -13.00000000000000178, 1.592040838891559293E-15, -58.22539674441618018 ) ) ;
#906 = CARTESIAN_POINT ( 'NONE',  ( 1.853537052132013807, -8.546502713975392851, 14.00000000000000000 ) ) ;
#907 = EDGE_LOOP ( 'NONE', ( #5557, #3894 ) ) ;
#908 = CARTESIAN_POINT ( 'NONE',  ( 3.605080641954653053, -9.570177220923548944, 1.999999999999998224 ) ) ;
#909 = CARTESIAN_POINT ( 'NONE',  ( -2.440069559021881496, 10.46881825416662259, 1.999999999999998224 ) ) ;
#910 = ADVANCED_FACE ( 'NONE', ( #5075 ), #4936, .F. ) ;
#911 = CARTESIAN_POINT ( 'NONE',  ( -7.227555219266157849, -1.939125212622549999, 13.99999999999999645 ) ) ;
#912 = ITEM_DEFINED_TRANSFORMATION ( 'NONE', 'NONE', #3428,  #1336 ) ;
#913 = CARTESIAN_POINT ( 'NONE',  ( -3.109042548464319378, -8.271822080922653697, 1.999999999999998224 ) ) ;
#914 = CARTESIAN_POINT ( 'NONE',  ( -4.372214883940050534, 6.312905667202751481, 1.999999999999998224 ) ) ;
#915 = DIRECTION ( 'NONE',  ( -0.000000000000000000, -0.000000000000000000, -1.000000000000000000 ) ) ;
#916 = EDGE_CURVE ( 'NONE', #1655, #5544, #2733, .T. ) ;
#917 = CARTESIAN_POINT ( 'NONE',  ( 0.000000000000000000, -0.7216878364870318308, -1.250000000000000000 ) ) ;
#918 =( NAMED_UNIT ( * ) PLANE_ANGLE_UNIT ( ) SI_UNIT ( $, .RADIAN. ) );
#919 = CARTESIAN_POINT ( 'NONE',  ( 4.513069810084762601, -3.445129632735342451, 1.999999999999998224 ) ) ;
#920 = CARTESIAN_POINT ( 'NONE',  ( 0.000000000000000000, 0.000000000000000000, -5.000000000000000000 ) ) ;
#921 = DIRECTION ( 'NONE',  ( 1.000000000000000000, 0.000000000000000000, 0.000000000000000000 ) ) ;
#922 = ORIENTED_EDGE ( 'NONE', *, *, #4867, .T. ) ;
#923 =( NAMED_UNIT ( * ) PLANE_ANGLE_UNIT ( ) SI_UNIT ( $, .RADIAN. ) );
#924 = FACE_OUTER_BOUND ( 'NONE', #1877, .T. ) ;
#925 = EDGE_CURVE ( 'NONE', #3736, #899, #5483, .T. ) ;
#926 = DIRECTION ( 'NONE',  ( -0.000000000000000000, -0.000000000000000000, 1.000000000000000000 ) ) ;
#927 = DIRECTION ( 'NONE',  ( 0.000000000000000000, 0.000000000000000000, 1.000000000000000000 ) ) ;
#928 = VERTEX_POINT ( 'NONE', #2463 ) ;
#929 = ORIENTED_EDGE ( 'NONE', *, *, #5527, .F. ) ;
#930 = CARTESIAN_POINT ( 'NONE',  ( -6.398096652174581678, -7.548242073784473760, 14.00000000000000000 ) ) ;
#931 = CARTESIAN_POINT ( 'NONE',  ( -7.521311085815506559, -0.1255077825093695587, 1.999999999999998224 ) ) ;
#932 = CARTESIAN_POINT ( 'NONE',  ( 5.059064342543293513, -7.053288479151686552, 1.999999999999998224 ) ) ;
#933 = CARTESIAN_POINT ( 'NONE',  ( -7.892574838092353495, -1.309761382309196032, 14.00000000000000000 ) ) ;
#934 = ORIENTED_EDGE ( 'NONE', *, *, #585, .F. ) ;
#935 = CARTESIAN_POINT ( 'NONE',  ( -3.798941939731882655, -9.621416145858376012, 1.999999999999998224 ) ) ;
#936 = PLANE ( 'NONE',  #4756 ) ;
#937 = EDGE_CURVE ( 'NONE', #2377, #1307, #3355, .T. ) ;
#938 = CARTESIAN_POINT ( 'NONE',  ( 3.426039378954557346, 5.938690629332270987, 13.99999999999999645 ) ) ;
#939 = CARTESIAN_POINT ( 'NONE',  ( 1.147089839255700294, -8.682979827541576157, 1.999999999999998224 ) ) ;
#940 = ORIENTED_EDGE ( 'NONE', *, *, #5169, .F. ) ;
#941 = PRESENTATION_LAYER_ASSIGNMENT (  '', '', ( #5073 ) ) ;
#942 = CARTESIAN_POINT ( 'NONE',  ( 3.892125705850321804, -6.036954802193386982, 1.999999999999998224 ) ) ;
#943 = CARTESIAN_POINT ( 'NONE',  ( -25.00000000000000000, 0.000000000000000000, 8.000000000000000000 ) ) ;
#944 = FACE_OUTER_BOUND ( 'NONE', #125, .T. ) ;
#945 = LINE ( 'NONE', #3506, #3628 ) ;
#946 =( LENGTH_UNIT ( ) NAMED_UNIT ( * ) SI_UNIT ( .MILLI., .METRE. ) );
#947 = CARTESIAN_POINT ( 'NONE',  ( -13.00000000000000178, 1.592040838891559293E-15, 12.00000000000000000 ) ) ;
#948 = DIRECTION ( 'NONE',  ( 0.000000000000000000, -1.000000000000000000, 0.000000000000000000 ) ) ;
#949 = CARTESIAN_POINT ( 'NONE',  ( 21.74999999999999645, -30.00000000000000000, 12.00000000000000000 ) ) ;
#950 = ORIENTED_EDGE ( 'NONE', *, *, #2485, .T. ) ;
#951 = EDGE_CURVE ( 'NONE', #3918, #1059, #3724, .T. ) ;
#952 = FILL_AREA_STYLE_COLOUR ( '', #59 ) ;
#953 = SHAPE_REPRESENTATION ( 'outer cover 2', ( #1336 ), #1859 ) ;
#954 = CARTESIAN_POINT ( 'NONE',  ( 17.55913978494622896, -14.85518798308249266, 8.000000000000000000 ) ) ;
#955 = DIRECTION ( 'NONE',  ( -0.000000000000000000, -0.000000000000000000, 1.000000000000000000 ) ) ;
#956 = EDGE_LOOP ( 'NONE', ( #1164, #1024 ) ) ;
#957 = CARTESIAN_POINT ( 'NONE',  ( 0.000000000000000000, 21.95856267278071527, 12.00000000000000000 ) ) ;
#958 = CARTESIAN_POINT ( 'NONE',  ( -10.03347820201837237, 0.3196629254998830660, 14.00000000000000000 ) ) ;
#959 = CARTESIAN_POINT ( 'NONE',  ( -7.227555219266156072, -1.939125212622417660, 1.999999999999998224 ) ) ;
#960 = VECTOR ( 'NONE', #1765, 999.9999999999998863 ) ;
#961 = CARTESIAN_POINT ( 'NONE',  ( -0.2798806129216870886, -8.779921314118375619, 1.999999999999998224 ) ) ;
#962 = ADVANCED_FACE ( 'NONE', ( #5049 ), #649, .T. ) ;
#963 = CARTESIAN_POINT ( 'NONE',  ( 7.379526280503350577, 5.862399640741291940, 14.00000000000000000 ) ) ;
#964 = VERTEX_POINT ( 'NONE', #4986 ) ;
#965 = CARTESIAN_POINT ( 'NONE',  ( -8.741731599017841248, 6.051300285686449953, 1.999999999999998224 ) ) ;
#966 = CARTESIAN_POINT ( 'NONE',  ( -1.336592501075063666, -5.709464570123372162, 14.00000000000000000 ) ) ;
#967 = CARTESIAN_POINT ( 'NONE',  ( -7.763712483375483586, -3.368527140561099031, 13.99999999999999645 ) ) ;
#968 = VECTOR ( 'NONE', #1615, 1000.000000000000000 ) ;
#969 = CARTESIAN_POINT ( 'NONE',  ( -7.521311085815508335, -0.1255077825093697530, 13.99999999999999645 ) ) ;
#970 = CARTESIAN_POINT ( 'NONE',  ( -7.304208470130000741, 7.056621303511527721, 1.999999999999998224 ) ) ;
#971 = ORIENTED_EDGE ( 'NONE', *, *, #1622, .T. ) ;
#972 = CIRCLE ( 'NONE', #3542, 5.000000000000000000 ) ;
#973 = CARTESIAN_POINT ( 'NONE',  ( 5.857810772706377733, -5.665644577056675679, 1.999999999999998224 ) ) ;
#974 = DIRECTION ( 'NONE',  ( 0.000000000000000000, 0.000000000000000000, -1.000000000000000000 ) ) ;
#975 = EDGE_CURVE ( 'NONE', #2597, #4467, #4617, .T. ) ;
#976 = LINE ( 'NONE', #3168, #5554 ) ;
#977 = CIRCLE ( 'NONE', #3188, 23.00000000000000000 ) ;
#978 = PLANE ( 'NONE',  #1040 ) ;
#979 = CARTESIAN_POINT ( 'NONE',  ( -6.048456868091350636, 0.8014113234715940504, 1.999999999999998224 ) ) ;
#980 = PLANE ( 'NONE',  #3743 ) ;
#981 = VECTOR ( 'NONE', #2742, 1000.000000000000000 ) ;
#982 = DIRECTION ( 'NONE',  ( 0.000000000000000000, 0.000000000000000000, -1.000000000000000000 ) ) ;
#983 = CARTESIAN_POINT ( 'NONE',  ( 7.456063200421762183, 7.959410280422752670, 13.99999999999999645 ) ) ;
#984 = VECTOR ( 'NONE', #3012, 1000.000000000000000 ) ;
#985 = PLANE ( 'NONE',  #5010 ) ;
#986 = ORIENTED_EDGE ( 'NONE', *, *, #1101, .T. ) ;
#987 = ORIENTED_EDGE ( 'NONE', *, *, #1553, .F. ) ;
#988 = CARTESIAN_POINT ( 'NONE',  ( -5.391417556047953141, 8.653185861734563389, 14.00000000000000000 ) ) ;
#989 = CARTESIAN_POINT ( 'NONE',  ( -6.762100275670003491, 3.470635719505328343, 1.999999999999998224 ) ) ;
#990 = AXIS2_PLACEMENT_3D ( 'NONE', #4490, #1470, #3658 ) ;
#991 = CARTESIAN_POINT ( 'NONE',  ( 3.810368753942602993, 7.433568398487427231, 1.999999999999998224 ) ) ;
#992 = CARTESIAN_POINT ( 'NONE',  ( -9.031632682309723492, 0.1436733667526614300, 14.00000000000000000 ) ) ;
#993 = VERTEX_POINT ( 'NONE', #5512 ) ;
#994 = CARTESIAN_POINT ( 'NONE',  ( -8.483256258862246213, -6.077987531410204980, 1.999999999999998224 ) ) ;
#995 = DIRECTION ( 'NONE',  ( -1.000000000000000000, -0.000000000000000000, -0.000000000000000000 ) ) ;
#996 = CARTESIAN_POINT ( 'NONE',  ( -5.741039858921713979, -6.128965587877692300, 13.99999999999999645 ) ) ;
#997 = CARTESIAN_POINT ( 'NONE',  ( -6.762100275670005267, 3.470635719505328787, 13.99999999999999645 ) ) ;
#998 = ADVANCED_FACE ( 'NONE', ( #2029 ), #2922, .F. ) ;
#999 = CARTESIAN_POINT ( 'NONE',  ( -1.320393794063943860, 6.095439640211754551, 14.00000000000000000 ) ) ;
#1000 = VERTEX_POINT ( 'NONE', #3784 ) ;
#1001 = EDGE_CURVE ( 'NONE', #4842, #1005, #1915, .T. ) ;
#1002 = CARTESIAN_POINT ( 'NONE',  ( 9.020117466466054168, 0.2947087185667776055, 1.999999999999998224 ) ) ;
#1003 = DIRECTION ( 'NONE',  ( 1.000000000000000000, 0.000000000000000000, 0.000000000000000000 ) ) ;
#1004 = CARTESIAN_POINT ( 'NONE',  ( 6.340368144647110071, -1.697206311170896598, 1.999999999999998224 ) ) ;
#1005 = VERTEX_POINT ( 'NONE', #2808 ) ;
#1006 = CARTESIAN_POINT ( 'NONE',  ( 5.195030181282357162, -4.117271336869386289, 1.999999999999998224 ) ) ;
#1007 = DIRECTION ( 'NONE',  ( -1.000000000000000000, 0.000000000000000000, 0.000000000000000000 ) ) ;
#1008 = ADVANCED_FACE ( 'NONE', ( #4558 ), #620, .T. ) ;
#1009 = FACE_BOUND ( 'NONE', #1425, .T. ) ;
#1010 = DIRECTION ( 'NONE',  ( -0.000000000000000000, -0.000000000000000000, 1.000000000000000000 ) ) ;
#1011 = CARTESIAN_POINT ( 'NONE',  ( 0.000000000000000000, 0.000000000000000000, -8.000000000000000000 ) ) ;
#1012 = VERTEX_POINT ( 'NONE', #4674 ) ;
#1013 = DIRECTION ( 'NONE',  ( -3.540989467475305966E-16, -1.000000000000000000, -0.000000000000000000 ) ) ;
#1014 = CARTESIAN_POINT ( 'NONE',  ( 9.123540010895988317, -2.926742269086383796, 14.00000000000000000 ) ) ;
#1015 = CARTESIAN_POINT ( 'NONE',  ( 2.321214644803172078, -6.838859567843806886, 1.999999999999998224 ) ) ;
#1016 = CARTESIAN_POINT ( 'NONE',  ( -8.290222237438479524, 3.747600907060152142, 1.999999999999998224 ) ) ;
#1017 = CARTESIAN_POINT ( 'NONE',  ( 4.853468040355885194, -8.397360160973688537, 14.00000000000000000 ) ) ;
#1018 = ORIENTED_EDGE ( 'NONE', *, *, #395, .F. ) ;
#1019 = CARTESIAN_POINT ( 'NONE',  ( -10.53467355221071777, 0.3418899515810866485, 1.999999999999998224 ) ) ;
#1020 = CARTESIAN_POINT ( 'NONE',  ( -1.320393794063943860, 6.095439640211754551, 14.00000000000000000 ) ) ;
#1021 = CARTESIAN_POINT ( 'NONE',  ( -3.441860715206332522, -7.602597312514155270, 13.99999999999999645 ) ) ;
#1022 = EDGE_CURVE ( 'NONE', #3723, #3918, #761, .T. ) ;
#1023 = CARTESIAN_POINT ( 'NONE',  ( 8.269507991092025279, 6.356934974247397285, 1.999999999999998224 ) ) ;
#1024 = ORIENTED_EDGE ( 'NONE', *, *, #1343, .T. ) ;
#1025 = CARTESIAN_POINT ( 'NONE',  ( -6.681468852107821377, -5.130140014479647625, 1.999999999999998224 ) ) ;
#1026 = FACE_OUTER_BOUND ( 'NONE', #3874, .T. ) ;
#1027 = CARTESIAN_POINT ( 'NONE',  ( -6.734745854535898246, 2.161492950161982396, 1.999999999999998224 ) ) ;
#1028 = VERTEX_POINT ( 'NONE', #2977 ) ;
#1029 = CARTESIAN_POINT ( 'NONE',  ( -2.717942380035140104, -6.274577315194988181, 1.999999999999998224 ) ) ;
#1030 = DIRECTION ( 'NONE',  ( 0.000000000000000000, 0.000000000000000000, 1.000000000000000000 ) ) ;
#1031 = DIRECTION ( 'NONE',  ( -0.000000000000000000, -0.000000000000000000, 1.000000000000000000 ) ) ;
#1032 = CARTESIAN_POINT ( 'NONE',  ( -6.762100275670003491, 3.470635719505328343, 1.999999999999998224 ) ) ;
#1033 = DIRECTION ( 'NONE',  ( -3.540989467475305966E-16, -1.000000000000000000, -0.000000000000000000 ) ) ;
#1034 = CYLINDRICAL_SURFACE ( 'NONE', #426, 23.00000000000000000 ) ;
#1035 = ORIENTED_EDGE ( 'NONE', *, *, #4653, .T. ) ;
#1036 = ADVANCED_FACE ( 'NONE', ( #5139, #844 ), #1284, .T. ) ;
#1037 = DIRECTION ( 'NONE',  ( 0.000000000000000000, 0.8660254037844387076, 0.4999999999999998890 ) ) ;
#1038 = CARTESIAN_POINT ( 'NONE',  ( -8.072272399573057200, -5.790267008922743486, 14.00000000000000000 ) ) ;
#1039 = CARTESIAN_POINT ( 'NONE',  ( -7.884571930971327802, 3.418633173532902969, 1.999999999999998224 ) ) ;
#1040 = AXIS2_PLACEMENT_3D ( 'NONE', #2620, #432, #2736 ) ;
#1041 = CARTESIAN_POINT ( 'NONE',  ( -8.999716648909558359, -0.5976852874978595409, 1.999999999999998224 ) ) ;
#1042 = CARTESIAN_POINT ( 'NONE',  ( 9.123540010895988317, -2.926742269086383796, 14.00000000000000000 ) ) ;
#1043 = FACE_OUTER_BOUND ( 'NONE', #2938, .T. ) ;
#1044 = ORIENTED_EDGE ( 'NONE', *, *, #653, .F. ) ;
#1045 = DIRECTION ( 'NONE',  ( 0.000000000000000000, 0.000000000000000000, -1.000000000000000000 ) ) ;
#1046 = CIRCLE ( 'NONE', #1974, 15.00000000000000000 ) ;
#1047 = CARTESIAN_POINT ( 'NONE',  ( 2.389076732465380548, -5.237771676862081449, 14.00000000000000000 ) ) ;
#1048 = CARTESIAN_POINT ( 'NONE',  ( -5.893815055328263774, 7.676334994785688259, 13.99999999999999645 ) ) ;
#1049 = CIRCLE ( 'NONE', #5651, 2.199999999999999289 ) ;
#1050 = CARTESIAN_POINT ( 'NONE',  ( -5.183646570197097958, -3.010418922386785212, 14.00000000000000000 ) ) ;
#1051 = ORIENTED_EDGE ( 'NONE', *, *, #3485, .T. ) ;
#1052 = CARTESIAN_POINT ( 'NONE',  ( -1.484422800923325125, -8.172499773499277254, 1.999999999999998224 ) ) ;
#1053=STYLED_ITEM('',(#5723),#2585);
#1054 = AXIS2_PLACEMENT_3D ( 'NONE', #2328, #1955, #1472 ) ;
#1055 = CARTESIAN_POINT ( 'NONE',  ( 0.000000000000000000, 0.000000000000000000, 15.94994774640597512 ) ) ;
#1056 = FILL_AREA_STYLE ('',( #3198 ) ) ;
#1057 = CARTESIAN_POINT ( 'NONE',  ( -0.8347742375825081274, 7.207659102801795115, 1.999999999999998224 ) ) ;
#1058 = VECTOR ( 'NONE', #1938, 1000.000000000000000 ) ;
#1059 = VERTEX_POINT ( 'NONE', #735 ) ;
#1060 = CARTESIAN_POINT ( 'NONE',  ( -0.8347742375825081274, 7.207659102801795115, 1.999999999999998224 ) ) ;
#1061 = PLANE ( 'NONE',  #3472 ) ;
#1062 = CARTESIAN_POINT ( 'NONE',  ( -22.50000000000000355, 0.000000000000000000, 14.00000000000000000 ) ) ;
#1063 = CIRCLE ( 'NONE', #1802, 25.00000000000000000 ) ;
#1064 = DIRECTION ( 'NONE',  ( 1.000000000000000000, 0.000000000000000000, 0.000000000000000000 ) ) ;
#1065 = DIRECTION ( 'NONE',  ( -1.000000000000000000, 0.000000000000000000, 0.000000000000000000 ) ) ;
#1066 = VECTOR ( 'NONE', #610, 1000.000000000000000 ) ;
#1067 = CARTESIAN_POINT ( 'NONE',  ( 2.200000000000000178, 4.653657836759941744E-16, -3.799999999999999378 ) ) ;
#1068 = ORIENTED_EDGE ( 'NONE', *, *, #1175, .F. ) ;
#1069 = CARTESIAN_POINT ( 'NONE',  ( -2.000000000000000000, 2.449293598294706414E-16, 4.000000000000000000 ) ) ;
#1070 = DIRECTION ( 'NONE',  ( 0.000000000000000000, -0.000000000000000000, -1.000000000000000000 ) ) ;
#1071 = CARTESIAN_POINT ( 'NONE',  ( 8.973806924230256499, -1.178693538871683488, 1.999999999999998224 ) ) ;
#1072 = CIRCLE ( 'NONE', #5025, 0.2000000000000000944 ) ;
#1073 = CARTESIAN_POINT ( 'NONE',  ( -3.672794075660469559, 8.451992513476518809, 1.999999999999998224 ) ) ;
#1074 = CARTESIAN_POINT ( 'NONE',  ( 9.527640065891670673, 0.1642265212908743666, 14.00000000000000000 ) ) ;
#1075 = CARTESIAN_POINT ( 'NONE',  ( 2.200000000000000622, 1.999999999999999112, 0.000000000000000000 ) ) ;
#1076 = ORIENTED_EDGE ( 'NONE', *, *, #2114, .F. ) ;
#1077 = DIRECTION ( 'NONE',  ( 0.000000000000000000, 0.000000000000000000, 1.000000000000000000 ) ) ;
#1078 = LINE ( 'NONE', #101, #1548 ) ;
#1079 = CARTESIAN_POINT ( 'NONE',  ( -3.290073422422831406, -8.739709727799914063, 13.99999999999999645 ) ) ;
#1080 = AXIS2_PLACEMENT_3D ( 'NONE', #5289, #3105, #5452 ) ;
#1081 = CARTESIAN_POINT ( 'NONE',  ( -7.559400777704422758, -6.425066744314571920, 1.999999999999998224 ) ) ;
#1082 = ORIENTED_EDGE ( 'NONE', *, *, #4109, .F. ) ;
#1083 = EDGE_CURVE ( 'NONE', #3693, #5521, #326, .T. ) ;
#1084 = CARTESIAN_POINT ( 'NONE',  ( 1.999247522871089311, 8.586038698136235325, 1.999999999999998224 ) ) ;
#1085 = CARTESIAN_POINT ( 'NONE',  ( 10.20000000000000107, 0.000000000000000000, 0.000000000000000000 ) ) ;
#1086 =( LENGTH_UNIT ( ) NAMED_UNIT ( * ) SI_UNIT ( .MILLI., .METRE. ) );
#1087 = CARTESIAN_POINT ( 'NONE',  ( -3.595699629853521984, 5.016010494498948091, 1.999999999999998224 ) ) ;
#1088 = ORIENTED_EDGE ( 'NONE', *, *, #2306, .T. ) ;
#1089 = CARTESIAN_POINT ( 'NONE',  ( 6.523553822664517554, -0.1051741892335503609, 1.999999999999998224 ) ) ;
#1090 = DIRECTION ( 'NONE',  ( 1.000000000000000000, 0.000000000000000000, 0.000000000000000000 ) ) ;
#1091 = DIRECTION ( 'NONE',  ( 0.000000000000000000, 0.000000000000000000, -1.000000000000000000 ) ) ;
#1092 = PRODUCT_DEFINITION_SHAPE ( 'NONE', 'NONE',  #5692 ) ;
#1093 = DIRECTION ( 'NONE',  ( -0.5000000000000044409, 0.000000000000000000, 0.8660254037844360431 ) ) ;
#1094 = EDGE_CURVE ( 'NONE', #300, #5686, #5596, .T. ) ;
#1095 = B_SPLINE_CURVE_WITH_KNOTS ( 'NONE', 3,
 ( #1611, #3369, #2525, #1181, #307, #3854, #5523, #3340, #5580, #5606, #2876, #1208, #4709, #3421, #1691, #1233, #4739, #2558, #692, #2445, #256, #2015, #1581, #5092, #2906, #1725, #3052, #1749, #2672, #4024, #4399, #80, #5293, #51, #3532, #4424, #3940, #1836, #3081, #454, #3026, #2185, #4796, #5239, #942, #1352, #1296, #1805, #4826, #2583, #5665, #5321, #3110, #857, #4373, #428, #3593, #4859, #1381, #478, #3136, #887, #2267, #2213, #4342, #1032, #3564, #3505, #4884, #914, #5264, #2236, #2647, #1264, #4771, #3964, #2696, #24, #4451, #831, #393, #2154, #1776, #1320, #2613, #3991, #512, #3910, #3477, #1946, #1893, #4080, #4913, #973, #2731, #2378, #133, #4483, #2291, #3649, #221, #1052, #540, #1977, #5431, #5458, #2814, #1025, #1486, #4993, #564, #5405, #1434, #3699, #4538, #106, #3220, #2407, #2845, #3193, #3275, #2783, #1514, #4051, #4566, #4168, #5027, #1084, #4597, #3675, #628, #1862, #4943, #3618, #656, #594, #5346, #2759, #1002, #1403, #5377, #3165, #4512, #2320, #1463, #4967, #4113, #2347, #166, #1920, #3245, #4138, #193, #5144, #799, #1174, #2552, #2060, #2518, #301, #1204, #5118, #2468, #1635, #3731, #4313, #4652, #5517, #2010, #3417, #3820, #3762, #4282, #1603, #5055, #2436, #2093, #5575, #1576, #1140, #2899, #2035, #3363, #2494, #5168, #5545, #2927, #4733, #4679, #1113, #719, #335, #4226, #3850, #3393, #277, #4705, #740, #5490, #1551, #4250, #5602, #2954, #767, #1661, #4623, #363, #1229, #3790, #3333, #5084, #2986, #3305, #2870, #683, #4199, #249, #1686, #3443, #5200, #4853, #1260, #827, #46, #3987, #3020, #909, #3936, #2668, #2120, #3875, #1345, #2641, #4765, #2579, #5317, #4337, #4395, #1315, #450, #2690, #852 ),
 .UNSPECIFIED., .F., .F.,
 ( 4, 2, 2, 2, 2, 2, 2, 2, 2, 2, 2, 2, 2, 2, 2, 2, 2, 2, 2, 2, 2, 2, 2, 2, 2, 2, 2, 2, 2, 2, 2, 2, 2, 2, 2, 2, 2, 2, 2, 2, 2, 2, 2, 2, 2, 2, 2, 2, 2, 2, 2, 2, 2, 2, 2, 2, 2, 2, 2, 2, 2, 2, 2, 2, 2, 2, 2, 2, 2, 2, 2, 2, 2, 2, 2, 2, 2, 2, 2, 2, 2, 2, 2, 2, 2, 2, 2, 2, 2, 2, 2, 2, 2, 2, 2, 2, 2, 2, 2, 2, 2, 2, 2, 2, 2, 2, 2, 2, 2, 2, 2, 2, 2, 2, 2, 2, 2, 2, 2, 2, 4 ),
 ( 0.000000000000000000, 0.01562500000000000000, 0.03125000000000000000, 0.04687500000000000000, 0.06250000000000000000, 0.07812500000000000000, 0.09375000000000000000, 0.1093750000000000000, 0.1250000000000000000, 0.1328125000000000000, 0.1406250000000000000, 0.1484375000000000000, 0.1562500000000000000, 0.1640625000000000000, 0.1718750000000000000, 0.1796875000000000000, 0.1875000000000000000, 0.1953125000000000000, 0.2031250000000000000, 0.2109375000000000000, 0.2187500000000000000, 0.2265625000000000000, 0.2343750000000000000, 0.2421875000000000000, 0.2500000000000000000, 0.2578125000000000000, 0.2656250000000000000, 0.2734375000000000000, 0.2812500000000000000, 0.2890625000000000000, 0.2968750000000000000, 0.3046875000000000000, 0.3125000000000000000, 0.3203125000000000000, 0.3281250000000000000, 0.3359375000000000000, 0.3437500000000000000, 0.3515625000000000000, 0.3593750000000000000, 0.3671875000000000000, 0.3750000000000000000, 0.3828125000000000000, 0.3906250000000000000, 0.3984375000000000000, 0.4062500000000000000, 0.4140625000000000000, 0.4218750000000000000, 0.4296875000000000000, 0.4375000000000000000, 0.4453125000000000000, 0.4531250000000000000, 0.4609375000000000000, 0.4687500000000000000, 0.4765625000000000000, 0.4843750000000000000, 0.4921875000000000000, 0.5000000000000000000, 0.5078125000000000000, 0.5156250000000000000, 0.5234375000000000000, 0.5312500000000000000, 0.5390625000000000000, 0.5468750000000000000, 0.5546875000000000000, 0.5625000000000000000, 0.5703125000000000000, 0.5781250000000000000, 0.5859375000000000000, 0.5937500000000000000, 0.6015625000000000000, 0.6093750000000000000, 0.6171875000000000000, 0.6250000000000000000, 0.6328125000000000000, 0.6406250000000000000, 0.6484375000000000000, 0.6562500000000000000, 0.6640625000000000000, 0.6718750000000000000, 0.6796875000000000000, 0.6875000000000000000, 0.6953125000000000000, 0.7031250000000000000, 0.7109375000000000000, 0.7187500000000000000, 0.7265625000000000000, 0.7343750000000000000, 0.7421875000000000000, 0.7500000000000000000, 0.7578125000000000000, 0.7656250000000000000, 0.7734375000000000000, 0.7812500000000000000, 0.7890625000000000000, 0.7968750000000000000, 0.8046875000000000000, 0.8125000000000000000, 0.8203125000000000000, 0.8281250000000000000, 0.8359375000000000000, 0.8437500000000000000, 0.8515625000000000000, 0.8593750000000000000, 0.8671875000000000000, 0.8750000000000000000, 0.8828125000000000000, 0.8906250000000000000, 0.8984375000000000000, 0.9062500000000000000, 0.9140625000000000000, 0.9218750000000000000, 0.9296875000000000000, 0.9375000000000000000, 0.9453125000000000000, 0.9531250000000000000, 0.9609375000000000000, 0.9687500000000000000, 0.9765625000000000000, 0.9843750000000000000, 0.9921875000000000000, 1.000000000000000000 ),
 .UNSPECIFIED. ) ;
#1096 = DIRECTION ( 'NONE',  ( -0.000000000000000000, 0.5000000000000001110, 0.8660254037844385966 ) ) ;
#1097 = ORIENTED_EDGE ( 'NONE', *, *, #1110, .F. ) ;
#1098 = LINE ( 'NONE', #2881, #331 ) ;
#1099 = CARTESIAN_POINT ( 'NONE',  ( 10.50003631213658117, 0.006025845833179007717, 14.00000000000000000 ) ) ;
#1100 = CARTESIAN_POINT ( 'NONE',  ( 1.954797901281672967, -9.037865403626939909, 1.999999999999998224 ) ) ;
#1101 = EDGE_CURVE ( 'NONE', #2131, #3736, #3831, .T. ) ;
#1102 = CARTESIAN_POINT ( 'NONE',  ( -7.884571930971329579, 3.418633173532294123, 13.99999999999999645 ) ) ;
#1103 = CARTESIAN_POINT ( 'NONE',  ( 0.000000000000000000, 0.000000000000000000, 2.000000000000000000 ) ) ;
#1104 = ORIENTED_EDGE ( 'NONE', *, *, #517, .F. ) ;
#1105 = LINE ( 'NONE', #4672, #511 ) ;
#1106 = ORIENTED_EDGE ( 'NONE', *, *, #4480, .T. ) ;
#1107 = CARTESIAN_POINT ( 'NONE',  ( 0.000000000000000000, 0.000000000000000000, 0.000000000000000000 ) ) ;
#1108 = CARTESIAN_POINT ( 'NONE',  ( 5.648567055624232225, 4.800053419556652656, 14.00000000000000000 ) ) ;
#1109 = CARTESIAN_POINT ( 'NONE',  ( -2.557952627993306471, -8.967547948949398773, 13.99999999999999645 ) ) ;
#1110 = EDGE_CURVE ( 'NONE', #3088, #5521, #1262, .T. ) ;
#1111 = CARTESIAN_POINT ( 'NONE',  ( 5.460516619045268527, 3.400499599735717915, 14.00000000000000000 ) ) ;
#1112 = ORIENTED_EDGE ( 'NONE', *, *, #3851, .F. ) ;
#1113 = CARTESIAN_POINT ( 'NONE',  ( 10.02932042447482175, 0.1670047327945775040, 1.999999999999998224 ) ) ;
#1114 = EDGE_CURVE ( 'NONE', #5601, #276, #2089, .T. ) ;
#1115 = DIRECTION ( 'NONE',  ( -0.000000000000000000, -0.000000000000000000, 1.000000000000000000 ) ) ;
#1116 = CARTESIAN_POINT ( 'NONE',  ( 1.730265954310492127, 6.073542049876722970, 1.999999999999998224 ) ) ;
#1117 = VERTEX_POINT ( 'NONE', #1252 ) ;
#1118 = CARTESIAN_POINT ( 'NONE',  ( -6.881333183080980298, -1.254343363641173381, 1.999999999999998224 ) ) ;
#1119 = DIRECTION ( 'NONE',  ( -1.000000000000000000, 0.000000000000000000, 0.000000000000000000 ) ) ;
#1120 = CARTESIAN_POINT ( 'NONE',  ( -1.451466707715608040, -6.203196315423898710, 13.99999999999999645 ) ) ;
#1121 = FACE_OUTER_BOUND ( 'NONE', #1958, .T. ) ;
#1122 = EDGE_CURVE ( 'NONE', #5494, #928, #1072, .T. ) ;
#1123 = CARTESIAN_POINT ( 'NONE',  ( -5.399999999999998579, 26.45448922205832787, 4.000000000000000000 ) ) ;
#1124 = EDGE_LOOP ( 'NONE', ( #4217, #5409, #2571, #1945 ) ) ;
#1125 = CYLINDRICAL_SURFACE ( 'NONE', #4289, 2.000000000000000000 ) ;
#1126 = CYLINDRICAL_SURFACE ( 'NONE', #1978, 3.799999999999999378 ) ;
#1127 = CARTESIAN_POINT ( 'NONE',  ( -8.388197440586290909, -1.387539741535495974, 1.999999999999998224 ) ) ;
#1128 = CARTESIAN_POINT ( 'NONE',  ( -1.565980662507674648, 8.609317438862776228, 13.99999999999999645 ) ) ;
#1129 = CARTESIAN_POINT ( 'NONE',  ( 1.837295235934470528, 10.14794156482770404, 14.00000000000000000 ) ) ;
#1130 = ORIENTED_EDGE ( 'NONE', *, *, #4867, .F. ) ;
#1131 = DIRECTION ( 'NONE',  ( -1.000000000000000000, 0.000000000000000000, 0.000000000000000000 ) ) ;
#1132 = EDGE_LOOP ( 'NONE', ( #2695, #837, #5190, #4747 ) ) ;
#1133 = CARTESIAN_POINT ( 'NONE',  ( 0.000000000000000000, 0.7216878364870328300, 1.249999999999999778 ) ) ;
#1134 = CARTESIAN_POINT ( 'NONE',  ( 6.268835244667308793, -4.335177162149436825, 14.00000000000000000 ) ) ;
#1135 = CARTESIAN_POINT ( 'NONE',  ( -9.406456921418632433, 1.708717176649267477, 13.99999999999999645 ) ) ;
#1136 = AXIS2_PLACEMENT_3D ( 'NONE', #2398, #707, #3382 ) ;
#1137 = CARTESIAN_POINT ( 'NONE',  ( 0.9466184546083361573, 7.233353930637703044, 14.00000000000000000 ) ) ;
#1138 = VECTOR ( 'NONE', #3169, 1000.000000000000000 ) ;
#1139 = VERTEX_POINT ( 'NONE', #5568 ) ;
#1140 = CARTESIAN_POINT ( 'NONE',  ( 3.158576809044846279, 9.313732666428188978, 1.999999999999998224 ) ) ;
#1141 = PRODUCT_DEFINITION_SHAPE ( 'NONE', 'NONE',  #5695 ) ;
#1142 = AXIS2_PLACEMENT_3D ( 'NONE', #5256, #2176, #2604 ) ;
#1143 = FACE_OUTER_BOUND ( 'NONE', #1789, .T. ) ;
#1144 = DIRECTION ( 'NONE',  ( 1.000000000000000000, 0.000000000000000000, 0.000000000000000000 ) ) ;
#1145 = CARTESIAN_POINT ( 'NONE',  ( -6.281085993838467552, -4.827840781182768382, 1.999999999999998224 ) ) ;
#1146 = ORIENTED_EDGE ( 'NONE', *, *, #3983, .F. ) ;
#1147 = CARTESIAN_POINT ( 'NONE',  ( -3.813875884798381577, -6.869235835554530212, 1.999999999999998224 ) ) ;
#1148 = AXIS2_PLACEMENT_3D ( 'NONE', #5005, #4577, #2387 ) ;
#1149 = EDGE_CURVE ( 'NONE', #2807, #1307, #2547, .T. ) ;
#1150 = CYLINDRICAL_SURFACE ( 'NONE', #4567, 25.00000000000000000 ) ;
#1151 = CARTESIAN_POINT ( 'NONE',  ( -2.122668041763332347, 7.434468402752584026, 13.99999999999999645 ) ) ;
#1152 = AXIS2_PLACEMENT_3D ( 'NONE', #4637, #2913, #3802 ) ;
#1153 = LINE ( 'NONE', #4124, #1162 ) ;
#1154 = CYLINDRICAL_SURFACE ( 'NONE', #882, 5.000000000000000000 ) ;
#1155 = ORIENTED_EDGE ( 'NONE', *, *, #4164, .T. ) ;
#1156 = VECTOR ( 'NONE', #2540, 999.9999999999998863 ) ;
#1157 = DIRECTION ( 'NONE',  ( 1.000000000000000000, 0.000000000000000000, 0.000000000000000000 ) ) ;
#1158 = DIRECTION ( 'NONE',  ( 0.000000000000000000, 0.000000000000000000, -1.000000000000000000 ) ) ;
#1159 = CARTESIAN_POINT ( 'NONE',  ( -6.681468852107821377, -5.130140014479647625, 1.999999999999998224 ) ) ;
#1160 = EDGE_CURVE ( 'NONE', #3604, #1139, #819, .T. ) ;
#1161 = CARTESIAN_POINT ( 'NONE',  ( 6.401046915552173644, 6.194151307163302533, 13.99999999999999645 ) ) ;
#1162 = VECTOR ( 'NONE', #666, 1000.000000000000000 ) ;
#1163 = CARTESIAN_POINT ( 'NONE',  ( 1.300000000000000044, -1.443375672974063884, -3.691112476943992763E-18 ) ) ;
#1164 = ORIENTED_EDGE ( 'NONE', *, *, #5104, .T. ) ;
#1165 = FACE_OUTER_BOUND ( 'NONE', #5587, .T. ) ;
#1166 = ORIENTED_EDGE ( 'NONE', *, *, #2730, .F. ) ;
#1167 = DIRECTION ( 'NONE',  ( -0.000000000000000000, 0.5000000000000001110, 0.8660254037844385966 ) ) ;
#1168 = CARTESIAN_POINT ( 'NONE',  ( 6.592258996018688144, -3.799026305082323418, 14.00000000000000000 ) ) ;
#1169 = CARTESIAN_POINT ( 'NONE',  ( 10.02239396097876423, -0.6576683464575836524, 13.99999999999999645 ) ) ;
#1170 = AXIS2_PLACEMENT_3D ( 'NONE', #4296, #838, #1701 ) ;
#1171 = CARTESIAN_POINT ( 'NONE',  ( 6.680730669075651385, 3.301097878975988831, 14.00000000000000000 ) ) ;
#1172 = AXIS2_PLACEMENT_3D ( 'NONE', #4145, #1091, #3312 ) ;
#1173 = ORIENTED_EDGE ( 'NONE', *, *, #1220, .F. ) ;
#1174 = CARTESIAN_POINT ( 'NONE',  ( -4.679820741051314847, -8.111215689328634681, 1.999999999999998224 ) ) ;
#1175 = EDGE_CURVE ( 'NONE', #3721, #1005, #1198, .T. ) ;
#1176 = VECTOR ( 'NONE', #5436, 1000.000000000000000 ) ;
#1177 = EDGE_CURVE ( 'NONE', #1387, #5593, #1996, .T. ) ;
#1178 = DIRECTION ( 'NONE',  ( 0.000000000000000000, 0.000000000000000000, -1.000000000000000000 ) ) ;
#1179 = DIRECTION ( 'NONE',  ( 0.000000000000000000, 0.000000000000000000, 1.000000000000000000 ) ) ;
#1180 = CARTESIAN_POINT ( 'NONE',  ( 7.526353627798827439, -0.2404185136226760222, 1.999999999999998224 ) ) ;
#1181 = CARTESIAN_POINT ( 'NONE',  ( 4.914575889516862972, -3.754581871930560144, 1.999999999999998224 ) ) ;
#1182 = CARTESIAN_POINT ( 'NONE',  ( 6.804422688527093754, 1.586354726854036112, 13.99999999999999645 ) ) ;
#1183 =( NAMED_UNIT ( * ) PLANE_ANGLE_UNIT ( ) SI_UNIT ( $, .RADIAN. ) );
#1184 = CARTESIAN_POINT ( 'NONE',  ( 7.258279873955303607, -6.354128476750924293, 1.999999999999998224 ) ) ;
#1185 = FACE_OUTER_BOUND ( 'NONE', #3674, .T. ) ;
#1186 = LINE ( 'NONE', #2075, #2523 ) ;
#1187 = ORIENTED_EDGE ( 'NONE', *, *, #3561, .T. ) ;
#1188 = DIRECTION ( 'NONE',  ( -0.000000000000000000, -0.000000000000000000, -1.000000000000000000 ) ) ;
#1189 = CARTESIAN_POINT ( 'NONE',  ( -4.500000000000000000, 5.510910596163088569E-16, -3.100000000000000533 ) ) ;
#1190 = CARTESIAN_POINT ( 'NONE',  ( -9.026614039607443019, -2.903226997913650465, 1.999999999999998224 ) ) ;
#1191 = EDGE_CURVE ( 'NONE', #4488, #1950, #3895, .T. ) ;
#1192 = CARTESIAN_POINT ( 'NONE',  ( 9.650319724629330409, 2.588775111615905011, 13.99999999999999645 ) ) ;
#1193 = CARTESIAN_POINT ( 'NONE',  ( 10.36702220812670028, 1.720931399333114120, 14.00000000000000000 ) ) ;
#1194 = VERTEX_POINT ( 'NONE', #5650 ) ;
#1195 = PRODUCT ( 'Spool Drum', 'Spool Drum', '', ( #4370 ) ) ;
#1196 = CYLINDRICAL_SURFACE ( 'NONE', #785, 22.50000000000000355 ) ;
#1197 = ORIENTED_EDGE ( 'NONE', *, *, #4090, .F. ) ;
#1198 = LINE ( 'NONE', #1680, #984 ) ;
#1199 = CARTESIAN_POINT ( 'NONE',  ( -6.065725208710916583, -3.376743199310593635, 14.00000000000000000 ) ) ;
#1200 = CARTESIAN_POINT ( 'NONE',  ( 5.279590631142085044, 9.498297537455629325, 13.99999999999999645 ) ) ;
#1201 = CARTESIAN_POINT ( 'NONE',  ( 7.526353627798829216, -0.2404185136226759112, 14.00000000000000000 ) ) ;
#1202 = ORIENTED_EDGE ( 'NONE', *, *, #3045, .F. ) ;
#1203 = EDGE_CURVE ( 'NONE', #4044, #4516, #2600, .T. ) ;
#1204 = CARTESIAN_POINT ( 'NONE',  ( -8.411612136543093143, -4.319922787977411360, 1.999999999999998224 ) ) ;
#1205 = DIRECTION ( 'NONE',  ( -1.000000000000000000, -0.000000000000000000, -0.000000000000000000 ) ) ;
#1206 = FILL_AREA_STYLE_COLOUR ( '', #3512 ) ;
#1207 = CARTESIAN_POINT ( 'NONE',  ( 7.439669587982602472, 0.9822684312230360870, 1.999999999999998224 ) ) ;
#1208 = CARTESIAN_POINT ( 'NONE',  ( -5.623512120026769701, -3.262381593762911258, 1.999999999999998224 ) ) ;
#1209 = CARTESIAN_POINT ( 'NONE',  ( 1.649120185255091187, 7.633850905136058351, 13.99999999999999645 ) ) ;
#1210 = SURFACE_SIDE_STYLE ('',( #3450 ) ) ;
#1211 = EDGE_CURVE ( 'NONE', #4096, #1000, #5227, .T. ) ;
#1212 = CARTESIAN_POINT ( 'NONE',  ( -1.515482495401827556, 9.129776367296644324, 1.999999999999998224 ) ) ;
#1213 = CARTESIAN_POINT ( 'NONE',  ( 10.20000000000000107, 0.000000000000000000, 1.610000000000000098 ) ) ;
#1214 = DIRECTION ( 'NONE',  ( 0.000000000000000000, -0.8660254037844385966, -0.5000000000000003331 ) ) ;
#1215 = ORIENTED_EDGE ( 'NONE', *, *, #3973, .F. ) ;
#1216 = DIRECTION ( 'NONE',  ( -1.000000000000000000, -0.000000000000000000, -0.000000000000000000 ) ) ;
#1217 = CARTESIAN_POINT ( 'NONE',  ( 0.000000000000000000, 0.000000000000000000, 24.08672805191341482 ) ) ;
#1218 = CARTESIAN_POINT ( 'NONE',  ( -1.592064345877354903, 9.625584969239746158, 13.99999999999999645 ) ) ;
#1219 = CARTESIAN_POINT ( 'NONE',  ( 6.452733273991772656, 8.145031704320798482, 14.00000000000000000 ) ) ;
#1220 = EDGE_CURVE ( 'NONE', #186, #300, #4785, .T. ) ;
#1221 = ORIENTED_EDGE ( 'NONE', *, *, #3980, .F. ) ;
#1222 = DIRECTION ( 'NONE',  ( -1.000000000000000000, -0.000000000000000000, -0.000000000000000000 ) ) ;
#1223 = ORIENTED_EDGE ( 'NONE', *, *, #3217, .T. ) ;
#1224 = DIRECTION ( 'NONE',  ( -1.000000000000000000, 0.000000000000000000, 0.000000000000000000 ) ) ;
#1225 = CARTESIAN_POINT ( 'NONE',  ( 7.526353627798829216, -0.2404185136226759112, 14.00000000000000000 ) ) ;
#1226 = CARTESIAN_POINT ( 'NONE',  ( 0.1774200004017887078, 10.78715707688374614, 13.99999999999999645 ) ) ;
#1227 = CARTESIAN_POINT ( 'NONE',  ( -6.317162512442926037, 3.238855812894408714, 14.00000000000000000 ) ) ;
#1228 = ORIENTED_EDGE ( 'NONE', *, *, #2292, .F. ) ;
#1229 = CARTESIAN_POINT ( 'NONE',  ( -6.045729098460860484, -8.441868823237593134, 1.999999999999998224 ) ) ;
#1230 = DIRECTION ( 'NONE',  ( -0.000000000000000000, -0.000000000000000000, -1.000000000000000000 ) ) ;
#1231 = AXIS2_PLACEMENT_3D ( 'NONE', #5535, #4721, #2082 ) ;
#1232 = CARTESIAN_POINT ( 'NONE',  ( -2.138212235155099616, 7.953261502403489835, 1.999999999999998224 ) ) ;
#1233 = CARTESIAN_POINT ( 'NONE',  ( -5.978927507574433697, 2.933119789328457294, 1.999999999999998224 ) ) ;
#1234 = CARTESIAN_POINT ( 'NONE',  ( 3.892125705850195683, -6.036954802193643665, 13.99999999999999645 ) ) ;
#1235 = CIRCLE ( 'NONE', #5096, 23.00000000000000000 ) ;
#1236 = CARTESIAN_POINT ( 'NONE',  ( -5.748891254250207083, -8.037420881456807109, 1.999999999999998224 ) ) ;
#1237 = CIRCLE ( 'NONE', #1785, 1.249999999999999778 ) ;
#1238 = CARTESIAN_POINT ( 'NONE',  ( 2.200000000000000178, 0.000000000000000000, 0.000000000000000000 ) ) ;
#1239 = CYLINDRICAL_SURFACE ( 'NONE', #3727, 25.00000000000000000 ) ;
#1240 = VERTEX_POINT ( 'NONE', #3493 ) ;
#1241 = FACE_BOUND ( 'NONE', #2539, .T. ) ;
#1242 = FACE_OUTER_BOUND ( 'NONE', #3299, .T. ) ;
#1243 = AXIS2_PLACEMENT_3D ( 'NONE', #5613, #2971, #4485 ) ;
#1244 = CARTESIAN_POINT ( 'NONE',  ( 3.388254439433305176, -8.575817650944683734, 13.99999999999999645 ) ) ;
#1245 = EDGE_CURVE ( 'NONE', #5361, #1550, #5253, .T. ) ;
#1246 = PLANE ( 'NONE',  #4536 ) ;
#1248 = EDGE_LOOP ( 'NONE', ( #492, #1082, #2541 ) ) ;
#1247 = AXIS2_PLACEMENT_3D ( 'NONE', #1760, #1390, #900 ) ;
#1249 = CARTESIAN_POINT ( 'NONE',  ( 0.000000000000000000, 0.000000000000000000, 4.000000000000000000 ) ) ;
#1250 = ADVANCED_FACE ( 'NONE', ( #2218 ), #1325, .F. ) ;
#1251 = VERTEX_POINT ( 'NONE', #893 ) ;
#1252 = CARTESIAN_POINT ( 'NONE',  ( -12.50000000000000000, 0.000000000000000000, 2.000000000000000000 ) ) ;
#1253 = CARTESIAN_POINT ( 'NONE',  ( -2.020383375745357313, -7.552201994671271734, 14.00000000000000000 ) ) ;
#1254 = CARTESIAN_POINT ( 'NONE',  ( 10.86297249782086105, 1.796588950249321304, 13.99999999999999645 ) ) ;
#1255 = UNCERTAINTY_MEASURE_WITH_UNIT (LENGTH_MEASURE( 1.000000000000000082E-05 ), #1086, 'distance_accuracy_value', 'NONE');
#1256 = CIRCLE ( 'NONE', #1987, 0.2000000000000000944 ) ;
#1257 = CARTESIAN_POINT ( 'NONE',  ( 4.415008247871436531, 7.106745273741267965, 14.00000000000000000 ) ) ;
#1258 = ORIENTED_EDGE ( 'NONE', *, *, #951, .F. ) ;
#1259 = CIRCLE ( 'NONE', #3647, 2.000000000000000000 ) ;
#1260 = CARTESIAN_POINT ( 'NONE',  ( -7.660583958272733973, 7.409732212660907535, 1.999999999999998224 ) ) ;
#1261 = CARTESIAN_POINT ( 'NONE',  ( 6.209839678909983895, -3.451293940533043614, 13.99999999999999645 ) ) ;
#1262 = CIRCLE ( 'NONE', #1808, 25.00000000000000000 ) ;
#1263 = CARTESIAN_POINT ( 'NONE',  ( -7.892574838092051515, -1.309761382309195366, 1.999999999999998224 ) ) ;
#1264 = CARTESIAN_POINT ( 'NONE',  ( -0.8890388043606449742, 7.706404363472288743, 1.999999999999998224 ) ) ;
#1265 = VECTOR ( 'NONE', #4458, 1000.000000000000227 ) ;
#1266 = CARTESIAN_POINT ( 'NONE',  ( -3.989331152809451275, -6.191695749071043586, 13.99999999999999645 ) ) ;
#1267 = DIRECTION ( 'NONE',  ( 0.000000000000000000, 0.000000000000000000, 1.000000000000000000 ) ) ;
#1268 =( LENGTH_UNIT ( ) NAMED_UNIT ( * ) SI_UNIT ( .MILLI., .METRE. ) );
#1269 = CARTESIAN_POINT ( 'NONE',  ( 6.863489721961431478, 6.439594285167053123, 1.999999999999998224 ) ) ;
#1270 = AXIS2_PLACEMENT_3D ( 'NONE', #1291, #3500, #3076 ) ;
#1271 = LINE ( 'NONE', #836, #5014 ) ;
#1272 = SURFACE_SIDE_STYLE ('',( #1646 ) ) ;
#1273 = ORIENTED_EDGE ( 'NONE', *, *, #3459, .T. ) ;
#1274 = EDGE_CURVE ( 'NONE', #2861, #1240, #2182, .T. ) ;
#1275 = DIRECTION ( 'NONE',  ( -1.000000000000000000, 0.000000000000000000, 0.000000000000000000 ) ) ;
#1276 = CARTESIAN_POINT ( 'NONE',  ( 0.000000000000000000, 0.000000000000000000, 2.000000000000000000 ) ) ;
#1277 = ADVANCED_FACE ( 'NONE', ( #4801 ), #980, .F. ) ;
#1278 = EDGE_CURVE ( 'NONE', #1594, #4303, #1732, .T. ) ;
#1279 = CARTESIAN_POINT ( 'NONE',  ( 9.843274586260610803, 1.790275038161259991, 13.99999999999999645 ) ) ;
#1280 = CARTESIAN_POINT ( 'NONE',  ( -5.000000000000076383, 22.44994432064363110, -8.000000000000000000 ) ) ;
#1281 = EDGE_LOOP ( 'NONE', ( #408, #5167, #940 ) ) ;
#1282 = FACE_OUTER_BOUND ( 'NONE', #5045, .T. ) ;
#1283 = VERTEX_POINT ( 'NONE', #5298 ) ;
#1284 = PLANE ( 'NONE',  #4206 ) ;
#1285 = CARTESIAN_POINT ( 'NONE',  ( 5.059064342543619475, -7.053288479152013402, 14.00000000000000000 ) ) ;
#1286 = EDGE_CURVE ( 'NONE', #4444, #1251, #4750, .T. ) ;
#1287 = CARTESIAN_POINT ( 'NONE',  ( -7.660583958272733973, 7.409732212661285011, 13.99999999999999645 ) ) ;
#1288 = PLANE ( 'NONE',  #3078 ) ;
#1289 = CARTESIAN_POINT ( 'NONE',  ( 8.453438707197836521, 0.9797652757261499090, 14.00000000000000000 ) ) ;
#1290 = ORIENTED_EDGE ( 'NONE', *, *, #4170, .F. ) ;
#1291 = CARTESIAN_POINT ( 'NONE',  ( 0.000000000000000000, 0.000000000000000000, 4.000000000000000000 ) ) ;
#1292 = CARTESIAN_POINT ( 'NONE',  ( -0.4015567206216588692, -6.330257989742014146, 13.99999999999999645 ) ) ;
#1293 = ITEM_DEFINED_TRANSFORMATION ( 'NONE', 'NONE', #2045,  #1336 ) ;
#1294 = CARTESIAN_POINT ( 'NONE',  ( 0.7514524083000287957, 9.263466152294371980, 1.999999999999998224 ) ) ;
#1295 = EDGE_CURVE ( 'NONE', #1815, #3046, #2550, .T. ) ;
#1296 = CARTESIAN_POINT ( 'NONE',  ( 2.321214644803172078, -6.838859567843806886, 1.999999999999998224 ) ) ;
#1297 = CARTESIAN_POINT ( 'NONE',  ( -3.594774944545354955, 7.935102286574237773, 13.99999999999999645 ) ) ;
#1298 = LINE ( 'NONE', #455, #1880 ) ;
#1299 = DIRECTION ( 'NONE',  ( 0.000000000000000000, 0.000000000000000000, -1.000000000000000000 ) ) ;
#1300 = LINE ( 'NONE', #5154, #4925 ) ;
#1301 = DIRECTION ( 'NONE',  ( -1.000000000000000000, 0.000000000000000000, 0.000000000000000000 ) ) ;
#1302 = EDGE_LOOP ( 'NONE', ( #5567, #2968, #2486, #718 ) ) ;
#1303 = CARTESIAN_POINT ( 'NONE',  ( 0.000000000000000000, 0.000000000000000000, -3.100000000000000533 ) ) ;
#1304 = CARTESIAN_POINT ( 'NONE',  ( -7.035243215357270152, 8.023489478516461659, 13.99999999999999645 ) ) ;
#1305 = VERTEX_POINT ( 'NONE', #29 ) ;
#1306 = CARTESIAN_POINT ( 'NONE',  ( -1.500000000000000888, 24.95495942693557012, 11.00000000000000000 ) ) ;
#1307 = VERTEX_POINT ( 'NONE', #5326 ) ;
#1308 = CARTESIAN_POINT ( 'NONE',  ( -5.399999999999998579, 26.45448922205832787, 12.00000000000000000 ) ) ;
#1309 = CARTESIAN_POINT ( 'NONE',  ( -1.390902631672706224, -7.679604985168660747, 14.00000000000000000 ) ) ;
#1310 = CARTESIAN_POINT ( 'NONE',  ( 6.000000000000000000, 0.000000000000000000, 1.999999999999998224 ) ) ;
#1311 = CARTESIAN_POINT ( 'NONE',  ( 13.00000000000000178, 0.000000000000000000, -58.22539674441618018 ) ) ;
#1312 = MECHANICAL_DESIGN_GEOMETRIC_PRESENTATION_REPRESENTATION (  '', ( #4977 ), #2871 ) ;
#1313 = CARTESIAN_POINT ( 'NONE',  ( 1.881113203117336319, 8.098457488330069509, 14.00000000000000000 ) ) ;
#1314 = ORIENTED_EDGE ( 'NONE', *, *, #1149, .T. ) ;
#1315 = CARTESIAN_POINT ( 'NONE',  ( 10.40193138080405255, 3.529992181067783452, 1.999999999999998224 ) ) ;
#1316 = CARTESIAN_POINT ( 'NONE',  ( -5.432680616552289621, 3.899654942172362748, 14.00000000000093792 ) ) ;
#1317 = APPLICATION_PROTOCOL_DEFINITION ( 'draft international standard', 'automotive_design', 1998, #2359 ) ;
#1318 = CARTESIAN_POINT ( 'NONE',  ( 5.710084532570392390, 7.448680193042510389, 1.999999999999998224 ) ) ;
#1319 = ORIENTED_EDGE ( 'NONE', *, *, #1160, .F. ) ;
#1320 = CARTESIAN_POINT ( 'NONE',  ( 7.132151089625187623, 3.519983721611797733, 1.999999999999998224 ) ) ;
#1321 = AXIS2_PLACEMENT_3D ( 'NONE', #84, #4799, #4376 ) ;
#1322 = DIRECTION ( 'NONE',  ( -1.000000000000000000, 0.000000000000000000, 0.000000000000000000 ) ) ;
#1323 = CARTESIAN_POINT ( 'NONE',  ( 6.452733273992156349, 8.145031704320794930, 1.999999999999998224 ) ) ;
#1324 = CARTESIAN_POINT ( 'NONE',  ( -5.637968025906138436, -2.116521738900817073, 1.999999999999998224 ) ) ;
#1325 = CYLINDRICAL_SURFACE ( 'NONE', #5398, 23.00000000000000000 ) ;
#1326 = VERTEX_POINT ( 'NONE', #2652 ) ;
#1327 = CARTESIAN_POINT ( 'NONE',  ( 0.000000000000000000, 4.653657836759941744E-16, -3.799999999999999378 ) ) ;
#1328 = AXIS2_PLACEMENT_3D ( 'NONE', #2036, #2064, #3821 ) ;
#1329 = CARTESIAN_POINT ( 'NONE',  ( -9.197478219253614640, 5.306711421960436326, 13.99999999999999645 ) ) ;
#1330 = DIRECTION ( 'NONE',  ( -1.156482317317871725E-16, -1.000000000000000000, 0.000000000000000000 ) ) ;
#1331 = ORIENTED_EDGE ( 'NONE', *, *, #446, .T. ) ;
#1332 = DIRECTION ( 'NONE',  ( -3.540989467475305966E-16, -1.000000000000000000, 0.000000000000000000 ) ) ;
#1333 = VERTEX_POINT ( 'NONE', #5245 ) ;
#1334 = PRESENTATION_LAYER_ASSIGNMENT (  '', '', ( #3266 ) ) ;
#1335 = DIRECTION ( 'NONE',  ( 1.000000000000000000, 0.000000000000000000, 0.000000000000000000 ) ) ;
#1336 = AXIS2_PLACEMENT_3D ( 'NONE', #283, #2997, #5213 ) ;
#1337 = CARTESIAN_POINT ( 'NONE',  ( -6.281085993838468440, -4.827840781183066809, 14.00000000000000000 ) ) ;
#1338 = CARTESIAN_POINT ( 'NONE',  ( -7.211577653563208123, 2.317451195016654530, 1.999999999999998224 ) ) ;
#1339 = VECTOR ( 'NONE', #4158, 1000.000000000000000 ) ;
#1340 = LINE ( 'NONE', #1311, #1873 ) ;
#1341 = CARTESIAN_POINT ( 'NONE',  ( -3.987536574861253236, 7.161134007378101352, 14.00000000000000000 ) ) ;
#1342 = ORIENTED_EDGE ( 'NONE', *, *, #4524, .F. ) ;
#1343 = EDGE_CURVE ( 'NONE', #1387, #5494, #5221, .T. ) ;
#1344 = CARTESIAN_POINT ( 'NONE',  ( 5.099673838352487998, -8.834479793761566668, 1.999999999999998224 ) ) ;
#1345 = CARTESIAN_POINT ( 'NONE',  ( 4.476660083460862971, 9.887553134099890784, 1.999999999999998224 ) ) ;
#1346 = CONICAL_SURFACE ( 'NONE', #4108, 2.000000000000000000, 1.029744258676656532 ) ;
#1347 = CARTESIAN_POINT ( 'NONE',  ( -3.989331152809451275, -6.191695749071043586, 13.99999999999999645 ) ) ;
#1348 = PRODUCT_CONTEXT ( 'NONE', #2952, 'mechanical' ) ;
#1349 = CARTESIAN_POINT ( 'NONE',  ( 8.618507686538960044, 3.909830026711944573, 1.999999999999998224 ) ) ;
#1350 = CIRCLE ( 'NONE', #5207, 25.00000000000000000 ) ;
#1351 = CIRCLE ( 'NONE', #4561, 15.00000000000000000 ) ;
#1352 = CARTESIAN_POINT ( 'NONE',  ( 2.869471237997587743, -6.613103333303327780, 1.999999999999998224 ) ) ;
#1353 = EDGE_CURVE ( 'NONE', #4627, #4235, #163, .T. ) ;
#1354 = PRESENTATION_LAYER_ASSIGNMENT (  '', '', ( #5488 ) ) ;
#1355 = DIRECTION ( 'NONE',  ( -0.000000000000000000, -0.000000000000000000, -1.000000000000000000 ) ) ;
#1356 = CARTESIAN_POINT ( 'NONE',  ( 5.326024957120312209, -1.813589758486610970, 1.999999999999998224 ) ) ;
#1357 = CIRCLE ( 'NONE', #1726, 13.00000000000000178 ) ;
#1358 = CARTESIAN_POINT ( 'NONE',  ( 5.733165789232423037, 2.946509839760266924, 1.999999999999998224 ) ) ;
#1359 = FACE_OUTER_BOUND ( 'NONE', #58, .T. ) ;
#1360 = EDGE_LOOP ( 'NONE', ( #1473, #179, #5383, #3317 ) ) ;
#1361 = LINE ( 'NONE', #1901, #4114 ) ;
#1362 = SHAPE_REPRESENTATION ( 'socket button head screw_iso_ISO 7380 - M4 x 8 - 8N', ( #1336 ), #5443 ) ;
#1363 = AXIS2_PLACEMENT_3D ( 'NONE', #3047, #2232, #4792 ) ;
#1364 = CARTESIAN_POINT ( 'NONE',  ( -9.742306995815035009, -3.848972158781221786, 13.99999999999999645 ) ) ;
#1365 = PLANE ( 'NONE',  #1599 ) ;
#1366 = CARTESIAN_POINT ( 'NONE',  ( 0.000000000000000000, 0.000000000000000000, 8.000000000000000000 ) ) ;
#1367 = ORIENTED_EDGE ( 'NONE', *, *, #5002, .T. ) ;
#1368 = EDGE_CURVE ( 'NONE', #4473, #118, #5491, .T. ) ;
#1369 = ORIENTED_EDGE ( 'NONE', *, *, #3787, .F. ) ;
#1370 = CARTESIAN_POINT ( 'NONE',  ( 8.618507686539667034, 3.909830026712121764, 14.00000000000000000 ) ) ;
#1371 = CARTESIAN_POINT ( 'NONE',  ( 2.869471237997587743, -6.613103333303327780, 1.999999999999998224 ) ) ;
#1372 = CARTESIAN_POINT ( 'NONE',  ( 6.929006764466009827, 4.804313515625705300, 1.999999999999998224 ) ) ;
#1373 = CARTESIAN_POINT ( 'NONE',  ( -7.425829140954380847, 3.215541426300493111, 14.00000000000000000 ) ) ;
#1374 = ORIENTED_EDGE ( 'NONE', *, *, #340, .T. ) ;
#1375 = CARTESIAN_POINT ( 'NONE',  ( 0.3355163285737912116, -10.27362971114624024, 1.999999999999998224 ) ) ;
#1376 = CARTESIAN_POINT ( 'NONE',  ( 25.00000000000000000, 3.061616997868383043E-15, 8.000000000000000000 ) ) ;
#1377 = CARTESIAN_POINT ( 'NONE',  ( 6.000000000000001776, 0.000000000000000000, 13.99999999999999645 ) ) ;
#1378 = APPLICATION_PROTOCOL_DEFINITION ( 'draft international standard', 'automotive_design', 1998, #3576 ) ;
#1379 = CARTESIAN_POINT ( 'NONE',  ( 0.3244988297792679166, -9.772062696132405080, 1.999999999999998224 ) ) ;
#1380 = EDGE_CURVE ( 'NONE', #5397, #1594, #4393, .T. ) ;
#1381 = CARTESIAN_POINT ( 'NONE',  ( -6.792624376349762905, -3.077375260546124203, 1.999999999999998224 ) ) ;
#1382 = LINE ( 'NONE', #1649, #3536 ) ;
#1383 = CARTESIAN_POINT ( 'NONE',  ( 0.000000000000000000, 0.000000000000000000, 12.00000000000000000 ) ) ;
#1384 = CARTESIAN_POINT ( 'NONE',  ( 9.925004466820084303, 3.374327561486830884, 1.999999999999998224 ) ) ;
#1385 = DIRECTION ( 'NONE',  ( -0.000000000000000000, -0.000000000000000000, 1.000000000000000000 ) ) ;
#1386 = CARTESIAN_POINT ( 'NONE',  ( 0.000000000000000000, 0.000000000000000000, 8.000000000000000000 ) ) ;
#1387 = VERTEX_POINT ( 'NONE', #2705 ) ;
#1388 = CARTESIAN_POINT ( 'NONE',  ( 17.99999999999999289, -17.34935157289748631, -8.000000000000000000 ) ) ;
#1389 = CARTESIAN_POINT ( 'NONE',  ( 9.599547022228486881, -3.085197981543154278, 13.99999999999999645 ) ) ;
#1390 = DIRECTION ( 'NONE',  ( 0.000000000000000000, 0.000000000000000000, -1.000000000000000000 ) ) ;
#1391 = EDGE_LOOP ( 'NONE', ( #1710, #4167, #3755, #5672, #2782 ) ) ;
#1392 = ORIENTED_EDGE ( 'NONE', *, *, #2121, .T. ) ;
#1393 = CARTESIAN_POINT ( 'NONE',  ( -4.354965481614498479, -8.841480220785717492, 14.00000000000000000 ) ) ;
#1394 = CARTESIAN_POINT ( 'NONE',  ( -5.322107489685658166, 5.499660323246576610, 1.999999999999998224 ) ) ;
#1395 = CARTESIAN_POINT ( 'NONE',  ( 3.857245400775495714, -7.804869966781508239, 1.999999999999998224 ) ) ;
#1396 = CARTESIAN_POINT ( 'NONE',  ( 2.992331685656917539, 8.840389773664524498, 14.00000000000000000 ) ) ;
#1397 = VERTEX_POINT ( 'NONE', #949 ) ;
#1398 = CARTESIAN_POINT ( 'NONE',  ( 10.02932042447482175, 0.1670047327945775040, 1.999999999999998224 ) ) ;
#1399 = DIRECTION ( 'NONE',  ( -0.000000000000000000, 0.4999999999999998890, -0.8660254037844387076 ) ) ;
#1400 = CARTESIAN_POINT ( 'NONE',  ( 7.992346231215207375, -0.9198489573344114101, 13.99999999999999645 ) ) ;
#1401 = CARTESIAN_POINT ( 'NONE',  ( -5.322107489685387272, 5.499660323246577498, 13.99999999999999645 ) ) ;
#1402 = CARTESIAN_POINT ( 'NONE',  ( 3.713512749562912774, 8.576920285552665391, 1.999999999999998224 ) ) ;
#1403 = CARTESIAN_POINT ( 'NONE',  ( 8.973806924230256499, -1.178693538871683488, 1.999999999999998224 ) ) ;
#1404 = CARTESIAN_POINT ( 'NONE',  ( 23.00000000000000000, -2.168404344971008868E-16, -16.41957833606399930 ) ) ;
#1405 = EDGE_CURVE ( 'NONE', #1005, #3984, #4403, .T. ) ;
#1406 = DIRECTION ( 'NONE',  ( -0.000000000000000000, -0.000000000000000000, 1.000000000000000000 ) ) ;
#1407 = AXIS2_PLACEMENT_3D ( 'NONE', #2555, #5549, #1606 ) ;
#1408 = PLANE ( 'NONE',  #1321 ) ;
#1409 = CARTESIAN_POINT ( 'NONE',  ( 0.2014543481397604585, 6.272771216426899166, 1.999999999999998224 ) ) ;
#1410 = CARTESIAN_POINT ( 'NONE',  ( -2.149999999999998579, 2.632990618166807756E-16, 0.000000000000000000 ) ) ;
#1411 = PRESENTATION_STYLE_ASSIGNMENT (( #4866 ) ) ;
#1412 = CARTESIAN_POINT ( 'NONE',  ( -3.287100391418014578, 10.22059872437975869, 13.99999999999999645 ) ) ;
#1413 = AXIS2_PLACEMENT_3D ( 'NONE', #3624, #3999, #2272 ) ;
#1414 =( NAMED_UNIT ( * ) SI_UNIT ( $, .STERADIAN. ) SOLID_ANGLE_UNIT ( ) );
#1415 = DIRECTION ( 'NONE',  ( -1.000000000000000000, 3.540989467475305966E-16, 0.000000000000000000 ) ) ;
#1416 = ORIENTED_EDGE ( 'NONE', *, *, #5052, .T. ) ;
#1417 = ORIENTED_EDGE ( 'NONE', *, *, #570, .F. ) ;
#1418 = CARTESIAN_POINT ( 'NONE',  ( 8.172274133038307298, -5.076547540501183065, 14.00000000000000000 ) ) ;
#1419 = CARTESIAN_POINT ( 'NONE',  ( 5.194219494279652238, 4.554949839096303243, 1.999999999999998224 ) ) ;
#1420 = AXIS2_PLACEMENT_3D ( 'NONE', #3872, #795, #4334 ) ;
#1421 = EDGE_CURVE ( 'NONE', #993, #5595, #459, .T. ) ;
#1422 = CARTESIAN_POINT ( 'NONE',  ( -2.415560149437878668, -8.486491385245608754, 1.999999999999998224 ) ) ;
#1423 = EDGE_CURVE ( 'NONE', #5009, #4159, #3539, .T. ) ;
#1424 = CARTESIAN_POINT ( 'NONE',  ( -7.161907081466633684, 5.673982509929174967, 14.00000000000000000 ) ) ;
#1425 = EDGE_LOOP ( 'NONE', ( #1744, #4928 ) ) ;
#1426 = CARTESIAN_POINT ( 'NONE',  ( -1.342170334697201595, -10.21728332006300199, 1.999999999999998224 ) ) ;
#1427 = CARTESIAN_POINT ( 'NONE',  ( 15.00000000000000000, 1.836970198721029589E-15, 4.000000000000000000 ) ) ;
#1428 = CARTESIAN_POINT ( 'NONE',  ( 8.952336951391263398, 1.032601321559317276, 13.99999999999999645 ) ) ;
#1429 = CIRCLE ( 'NONE', #5468, 4.500000000000000000 ) ;
#1430 = CARTESIAN_POINT ( 'NONE',  ( -0.2539011084976132149, 7.766605221862832309, 13.99999999999999645 ) ) ;
#1431 = CARTESIAN_POINT ( 'NONE',  ( -2.744490807750914918, 5.556819979548927257, 14.00000000000000000 ) ) ;
#1432 = ORIENTED_EDGE ( 'NONE', *, *, #6, .T. ) ;
#1433 = VECTOR ( 'NONE', #1967, 1000.000000000000000 ) ;
#1434 = CARTESIAN_POINT ( 'NONE',  ( -8.486979168634645632, -0.6954046021538184963, 1.999999999999998224 ) ) ;
#1435 = ADVANCED_FACE ( 'NONE', ( #1359 ), #4864, .F. ) ;
#1436 = CARTESIAN_POINT ( 'NONE',  ( 0.000000000000000000, 0.000000000000000000, -5.000000000000000000 ) ) ;
#1437 = LINE ( 'NONE', #1464, #2063 ) ;
#1438 = AXIS2_PLACEMENT_3D ( 'NONE', #56, #948, #4057 ) ;
#1439 = CARTESIAN_POINT ( 'NONE',  ( 6.004028658818956643, -2.715480180205985583, 1.999999999999998224 ) ) ;
#1440 = EDGE_LOOP ( 'NONE', ( #3729, #3554, #4497, #1761, #1130, #655 ) ) ;
#1441 = LINE ( 'NONE', #5325, #4078 ) ;
#1442 = CARTESIAN_POINT ( 'NONE',  ( -23.00000000000000000, 0.000000000000000000, -8.000000000000000000 ) ) ;
#1443 = AXIS2_PLACEMENT_3D ( 'NONE', #4550, #4182, #234 ) ;
#1444 = CARTESIAN_POINT ( 'NONE',  ( -6.112420884766619267, -2.295018720694776970, 13.99999999999999645 ) ) ;
#1445 = PLANE ( 'NONE',  #1148 ) ;
#1446 = SURFACE_STYLE_FILL_AREA ( #1929 ) ;
#1447 = PRODUCT_DEFINITION ( 'UNKNOWN', '', #5080, #1714 ) ;
#1448 = CARTESIAN_POINT ( 'NONE',  ( 1.300000000000000044, 0.000000000000000000, 0.000000000000000000 ) ) ;
#1449 = VERTEX_POINT ( 'NONE', #4429 ) ;
#1450 = PLANE ( 'NONE',  #2788 ) ;
#1451 = CARTESIAN_POINT ( 'NONE',  ( 9.164356920906893578, 2.464151434935829332, 14.00000000000000000 ) ) ;
#1452 = CARTESIAN_POINT ( 'NONE',  ( 5.213743241621227931, -4.883528188333804643, 1.999999999999998224 ) ) ;
#1453 = AXIS2_PLACEMENT_3D ( 'NONE', #5634, #2932, #2038 ) ;
#1454 = EDGE_CURVE ( 'NONE', #1655, #30, #4000, .T. ) ;
#1455 = CARTESIAN_POINT ( 'NONE',  ( -6.826495404309643966, 4.393449859560456083, 1.999999999999998224 ) ) ;
#1456 = CARTESIAN_POINT ( 'NONE',  ( 1.511842404626676961, 9.183516746439467582, 14.00000000000000000 ) ) ;
#1457 = ORIENTED_EDGE ( 'NONE', *, *, #5077, .F. ) ;
#1458 = CARTESIAN_POINT ( 'NONE',  ( 7.066195124645999748, -7.302433507960749637, 1.999999999999998224 ) ) ;
#1459 = CARTESIAN_POINT ( 'NONE',  ( -6.069783318623454882, -0.2142533344233820691, 14.00000000000000000 ) ) ;
#1460 = CARTESIAN_POINT ( 'NONE',  ( 8.027649061864064350, -0.2602747315786822502, 13.99999999999999645 ) ) ;
#1461 = CARTESIAN_POINT ( 'NONE',  ( 7.108868828250527905, 7.597268273414325535, 1.999999999999998224 ) ) ;
#1462 = VERTEX_POINT ( 'NONE', #3572 ) ;
#1463 = CARTESIAN_POINT ( 'NONE',  ( 6.971023843911450690, -5.915260676233723203, 1.999999999999998224 ) ) ;
#1464 = CARTESIAN_POINT ( 'NONE',  ( -2.000000000000000000, 2.449293598294706414E-16, 4.000000000000000000 ) ) ;
#1465 = FILL_AREA_STYLE_COLOUR ( '', #3791 ) ;
#1466 = CARTESIAN_POINT ( 'NONE',  ( 5.460516619045266751, 3.400499599735594014, 1.999999999999998224 ) ) ;
#1467 = ADVANCED_FACE ( 'NONE', ( #86 ), #1841, .F. ) ;
#1468 = ORIENTED_EDGE ( 'NONE', *, *, #752, .T. ) ;
#1469 = CARTESIAN_POINT ( 'NONE',  ( -6.742266116715657454, -1.811900715329134215, 1.999999999999998224 ) ) ;
#1470 = DIRECTION ( 'NONE',  ( 0.000000000000000000, 0.000000000000000000, 1.000000000000000000 ) ) ;
#1471 = CARTESIAN_POINT ( 'NONE',  ( 4.914575889516433094, -3.754581871930561032, 13.99999999999999645 ) ) ;
#1472 = DIRECTION ( 'NONE',  ( 1.000000000000000000, 0.000000000000000000, 0.000000000000000000 ) ) ;
#1473 = ORIENTED_EDGE ( 'NONE', *, *, #3717, .T. ) ;
#1474 = DIRECTION ( 'NONE',  ( 1.000000000000000000, 0.000000000000000000, 0.000000000000000000 ) ) ;
#1475 = CARTESIAN_POINT ( 'NONE',  ( 9.348788865899230416, 1.705571004836294646, 14.00000000000000000 ) ) ;
#1476 = CARTESIAN_POINT ( 'NONE',  ( -2.153669193480073574, -8.035861145135083206, 1.999999999999998224 ) ) ;
#1477 = CARTESIAN_POINT ( 'NONE',  ( 7.017208779832875720, -5.019401656906101294, 1.999999999999998224 ) ) ;
#1478 = CARTESIAN_POINT ( 'NONE',  ( -2.970508497641844325, 8.737606122599315128, 14.00000000000000000 ) ) ;
#1479 = LINE ( 'NONE', #3236, #1433 ) ;
#1480 = ORIENTED_EDGE ( 'NONE', *, *, #3678, .F. ) ;
#1481 = DIRECTION ( 'NONE',  ( -1.000000000000000000, 0.000000000000000000, 0.000000000000000000 ) ) ;
#1482 = CARTESIAN_POINT ( 'NONE',  ( 3.622712361020366867, 5.236663886535375845, 14.00000000000000000 ) ) ;
#1483 = CARTESIAN_POINT ( 'NONE',  ( -1.484422800923361985, -8.172499773498691056, 13.99999999999999645 ) ) ;
#1484 = CARTESIAN_POINT ( 'NONE',  ( 8.774740126074938473, 5.663528079765400847, 1.999999999999998224 ) ) ;
#1485 = ORIENTED_EDGE ( 'NONE', *, *, #3217, .F. ) ;
#1486 = CARTESIAN_POINT ( 'NONE',  ( -7.091148812992122963, -4.571561645352110403, 1.999999999999998224 ) ) ;
#1487 = DIRECTION ( 'NONE',  ( -1.000000000000000000, 0.000000000000000000, 0.000000000000000000 ) ) ;
#1488 = CARTESIAN_POINT ( 'NONE',  ( 4.062840028443489793, -5.287223670286648414, 1.999999999999998224 ) ) ;
#1489 = ORIENTED_EDGE ( 'NONE', *, *, #1353, .T. ) ;
#1490 = CARTESIAN_POINT ( 'NONE',  ( -7.019651866617071079, -0.1200674265790944856, 1.999999999999998224 ) ) ;
#1491 = DIRECTION ( 'NONE',  ( 0.000000000000000000, 0.000000000000000000, -1.000000000000000000 ) ) ;
#1492 = CARTESIAN_POINT ( 'NONE',  ( 5.806279480218260680, -1.975834710110475401, 13.99999999999999645 ) ) ;
#1493 = LINE ( 'NONE', #3742, #4639 ) ;
#1494 = DIRECTION ( 'NONE',  ( 0.000000000000000000, 0.000000000000000000, 1.000000000000000000 ) ) ;
#1495 = FACE_OUTER_BOUND ( 'NONE', #3746, .T. ) ;
#1496 = VERTEX_POINT ( 'NONE', #2353 ) ;
#1497 = DIRECTION ( 'NONE',  ( 0.06000000000000008105, -0.9981983770774224274, 0.000000000000000000 ) ) ;
#1498 = DIRECTION ( 'NONE',  ( -0.000000000000000000, -0.000000000000000000, -1.000000000000000000 ) ) ;
#1499 = CARTESIAN_POINT ( 'NONE',  ( 7.748217264256983761, 4.472783157626249562, 1.999999999999998224 ) ) ;
#1500 = CIRCLE ( 'NONE', #2792, 13.00000000000000178 ) ;
#1501 = CARTESIAN_POINT ( 'NONE',  ( 0.7514524083000287957, 9.263466152294371980, 1.999999999999998224 ) ) ;
#1502 = CARTESIAN_POINT ( 'NONE',  ( 5.071900148311402567, 7.881338450277072027, 14.00000000000000000 ) ) ;
#1503 = FACE_BOUND ( 'NONE', #956, .T. ) ;
#1504 = ORIENTED_EDGE ( 'NONE', *, *, #4283, .F. ) ;
#1505 = CARTESIAN_POINT ( 'NONE',  ( 6.769338797470902946, 8.534199679356609280, 1.999999999999998224 ) ) ;
#1506 = AXIS2_PLACEMENT_3D ( 'NONE', #4400, #1267, #4798 ) ;
#1507 = CARTESIAN_POINT ( 'NONE',  ( -5.000000000000000000, 4.999999999999978684, -5.000000000000000000 ) ) ;
#1508 = CARTESIAN_POINT ( 'NONE',  ( 6.019515613300196577, 7.843576796802396167, 13.99999999999999645 ) ) ;
#1509 = CIRCLE ( 'NONE', #777, 23.00000000000000000 ) ;
#1510 = EDGE_CURVE ( 'NONE', #1733, #4303, #3681, .T. ) ;
#1511 = CARTESIAN_POINT ( 'NONE',  ( -3.922355934210178585, -4.464780306277046584, 14.00000000000000000 ) ) ;
#1512 = APPLICATION_CONTEXT ( 'automotive_design' ) ;
#1513 = ORIENTED_EDGE ( 'NONE', *, *, #5599, .T. ) ;
#1514 = CARTESIAN_POINT ( 'NONE',  ( -3.594774944545354511, 7.935102286573618713, 1.999999999999998224 ) ) ;
#1515 = CIRCLE ( 'NONE', #1152, 23.00000000000000000 ) ;
#1516 = ADVANCED_FACE ( 'NONE', ( #2325 ), #2921, .F. ) ;
#1517 = CARTESIAN_POINT ( 'NONE',  ( 1.300000000000000044, 1.443375672974065216, 7.017607234860990640E-28 ) ) ;
#1518 = PRESENTATION_STYLE_ASSIGNMENT (( #5461 ) ) ;
#1519 = CARTESIAN_POINT ( 'NONE',  ( -5.525185448606692695, 2.707100724334796649, 1.999999999999998224 ) ) ;
#1520 = VECTOR ( 'NONE', #1332, 1000.000000000000000 ) ;
#1521 = ORIENTED_EDGE ( 'NONE', *, *, #4924, .F. ) ;
#1522 = CARTESIAN_POINT ( 'NONE',  ( 7.280083392764698402, -2.072676875633882254, 1.999999999999998224 ) ) ;
#1523 = DIRECTION ( 'NONE',  ( 1.000000000000000000, 0.000000000000000000, 0.000000000000000000 ) ) ;
#1524 = EDGE_CURVE ( 'NONE', #5544, #2880, #4972, .T. ) ;
#1525 = CARTESIAN_POINT ( 'NONE',  ( 0.000000000000000000, 0.000000000000000000, -8.000000000000000000 ) ) ;
#1526 = CONICAL_SURFACE ( 'NONE', #1895, 1.610000000000000098, 0.7853981633974458365 ) ;
#1527 = CARTESIAN_POINT ( 'NONE',  ( -1.380000000000002558, 21.95856267278071527, 12.00000000000000000 ) ) ;
#1528 = AXIS2_PLACEMENT_3D ( 'NONE', #2132, #2912, #2480 ) ;
#1529 = DIRECTION ( 'NONE',  ( 0.000000000000000000, 0.000000000000000000, -1.000000000000000000 ) ) ;
#1530 = EDGE_CURVE ( 'NONE', #1117, #4802, #2739, .T. ) ;
#1531 = ORIENTED_EDGE ( 'NONE', *, *, #4413, .F. ) ;
#1532 = CARTESIAN_POINT ( 'NONE',  ( 1.300000000000000044, -0.7216878364870318308, -1.250000000000000000 ) ) ;
#1533 = CARTESIAN_POINT ( 'NONE',  ( 0.000000000000000000, 0.000000000000000000, 8.000000000000000000 ) ) ;
#1534 = CARTESIAN_POINT ( 'NONE',  ( -6.848710654519973851, 5.255840572796829591, 1.999999999999998224 ) ) ;
#1535 = CLOSED_SHELL ( 'NONE', ( #2866, #5174, #4061, #4351, #5113, #4620, #3495, #398, #2220, #509, #5195, #4989, #1008, #3147, #1277, #2437, #5438 ) ) ;
#1536 = AXIS2_PLACEMENT_3D ( 'NONE', #3659, #1031, #3741 ) ;
#1537 = CARTESIAN_POINT ( 'NONE',  ( 0.5432484998931954578, -8.249156888542636068, 13.99999999999999645 ) ) ;
#1538 = CARTESIAN_POINT ( 'NONE',  ( 9.320190601379009010, -2.164585516638707574, 1.999999999999998224 ) ) ;
#1539 = DIRECTION ( 'NONE',  ( 0.000000000000000000, 0.000000000000000000, -1.000000000000000000 ) ) ;
#1540 = EDGE_CURVE ( 'NONE', #3849, #354, #342, .T. ) ;
#1541 = ORIENTED_EDGE ( 'NONE', *, *, #3983, .T. ) ;
#1542 = CARTESIAN_POINT ( 'NONE',  ( -25.00000000000000000, 0.000000000000000000, 8.000000000000000000 ) ) ;
#1543 = ORIENTED_EDGE ( 'NONE', *, *, #5588, .T. ) ;
#1544 = AXIS2_PLACEMENT_3D ( 'NONE', #3311, #3252, #4121 ) ;
#1545 = PLANE ( 'NONE',  #5581 ) ;
#1546 = CARTESIAN_POINT ( 'NONE',  ( 4.776808680784973227, 5.634249062854204126, 14.00000000000000000 ) ) ;
#1547 = CARTESIAN_POINT ( 'NONE',  ( 7.422282976138728117, -5.315384720684047437, 13.99999999999999645 ) ) ;
#1548 = VECTOR ( 'NONE', #1399, 1000.000000000000114 ) ;
#1549 = CARTESIAN_POINT ( 'NONE',  ( 2.672042568001582907, -6.151894458592797932, 14.00000000000000000 ) ) ;
#1550 = VERTEX_POINT ( 'NONE', #546 ) ;
#1551 = CARTESIAN_POINT ( 'NONE',  ( 3.605080641954653053, -9.570177220923548944, 1.999999999999998224 ) ) ;
#1552 = CARTESIAN_POINT ( 'NONE',  ( -15.00000000000000000, 0.000000000000000000, 4.000000000000000000 ) ) ;
#1553 = EDGE_CURVE ( 'NONE', #2807, #3887, #3203, .T. ) ;
#1554 =( LENGTH_UNIT ( ) NAMED_UNIT ( * ) SI_UNIT ( .MILLI., .METRE. ) );
#1555 = CARTESIAN_POINT ( 'NONE',  ( 0.5542950790998156796, -6.736796398737814329, 1.999999999999998224 ) ) ;
#1556 = VERTEX_POINT ( 'NONE', #1869 ) ;
#1557 = CARTESIAN_POINT ( 'NONE',  ( 1.760389272475360256, -7.536528230137968798, 1.999999999999998224 ) ) ;
#1558 = CARTESIAN_POINT ( 'NONE',  ( 0.000000000000000000, 0.000000000000000000, 2.000000000000000000 ) ) ;
#1559 = CARTESIAN_POINT ( 'NONE',  ( 1.380000000000002336, 22.95856267278071172, 15.94994774640597512 ) ) ;
#1560 = ADVANCED_FACE ( 'NONE', ( #4058 ), #5467, .T. ) ;
#1561 = PLANE ( 'NONE',  #3730 ) ;
#1562 = ORIENTED_EDGE ( 'NONE', *, *, #4062, .F. ) ;
#1563 = DIRECTION ( 'NONE',  ( 1.000000000000000000, 0.000000000000000000, 0.000000000000000000 ) ) ;
#1564 = DIRECTION ( 'NONE',  ( -1.000000000000000000, -0.000000000000000000, -0.000000000000000000 ) ) ;
#1565 = CARTESIAN_POINT ( 'NONE',  ( 4.074896204546095468, -8.256886768008961042, 1.999999999999998224 ) ) ;
#1566 = CARTESIAN_POINT ( 'NONE',  ( -4.227552200850896114, 7.601683304540504338, 13.99999999999999645 ) ) ;
#1567 = CARTESIAN_POINT ( 'NONE',  ( 8.673617379884035472E-16, -1.899999999999999689, -3.490243377569955075E-16 ) ) ;
#1568 = ORIENTED_EDGE ( 'NONE', *, *, #4598, .T. ) ;
#1569 = DIRECTION ( 'NONE',  ( 0.000000000000000000, 0.000000000000000000, 1.000000000000000000 ) ) ;
#1570 = EDGE_LOOP ( 'NONE', ( #4840, #1897, #4181, #4871 ) ) ;
#1571 = DIRECTION ( 'NONE',  ( -1.156482317317871478E-16, -1.000000000000000000, 0.000000000000000000 ) ) ;
#1572 = CARTESIAN_POINT ( 'NONE',  ( -5.370374743919055227, 4.702532619530572333, 14.00000000000000000 ) ) ;
#1573 = CARTESIAN_POINT ( 'NONE',  ( 7.775655769254120386, 6.170250810330326630, 13.99999999999999645 ) ) ;
#1574 = CARTESIAN_POINT ( 'NONE',  ( -5.370374743919055227, 4.702532619530572333, 14.00000000000000000 ) ) ;
#1575 = ORIENTED_EDGE ( 'NONE', *, *, #4653, .F. ) ;
#1576 = CARTESIAN_POINT ( 'NONE',  ( 1.598519525623709248, 9.677660462521251006, 1.999999999999998224 ) ) ;
#1577 = FACE_OUTER_BOUND ( 'NONE', #5516, .T. ) ;
#1578 = CARTESIAN_POINT ( 'NONE',  ( 3.520917041835318173, -6.848083076130971669, 1.999999999999998224 ) ) ;
#1579 = ORIENTED_EDGE ( 'NONE', *, *, #2603, .F. ) ;
#1580 = CARTESIAN_POINT ( 'NONE',  ( -1.390902631672706002, -7.679604985168658970, 1.999999999999998224 ) ) ;
#1581 = CARTESIAN_POINT ( 'NONE',  ( -0.8811140424828312057, 6.693995663234410642, 1.999999999999998224 ) ) ;
#1582 = CARTESIAN_POINT ( 'NONE',  ( -3.886954398759500773, 5.424498719065526053, 13.99999999999999645 ) ) ;
#1583 = STYLED_ITEM ( 'NONE', ( #4887 ), #1852 ) ;
#1584 = FILL_AREA_STYLE_COLOUR ( '', #3537 ) ;
#1585 = DIRECTION ( 'NONE',  ( -0.000000000000000000, -0.000000000000000000, -1.000000000000000000 ) ) ;
#1586 = ORIENTED_EDGE ( 'NONE', *, *, #364, .F. ) ;
#1587 = CARTESIAN_POINT ( 'NONE',  ( 1.300000000000000044, -0.7216878364870318308, 1.249999999999999778 ) ) ;
#1588 = CARTESIAN_POINT ( 'NONE',  ( 0.000000000000000000, 0.000000000000000000, 4.000000000000000000 ) ) ;
#1589 = CARTESIAN_POINT ( 'NONE',  ( -8.513020831365363250, 0.6954046021538080602, 1.999999999999998224 ) ) ;
#1590 = CARTESIAN_POINT ( 'NONE',  ( -7.211577653563209900, 2.317451195016654975, 13.99999999999999645 ) ) ;
#1591 = CARTESIAN_POINT ( 'NONE',  ( 2.667884741302309681, 9.975564253400266423, 14.00000000000000000 ) ) ;
#1592 = ORIENTED_EDGE ( 'NONE', *, *, #530, .F. ) ;
#1593 = DIRECTION ( 'NONE',  ( -1.000000000000000000, 0.000000000000000000, -0.000000000000000000 ) ) ;
#1594 = VERTEX_POINT ( 'NONE', #3626 ) ;
#1595 = DIRECTION ( 'NONE',  ( 1.000000000000000000, 0.000000000000000000, 0.000000000000000000 ) ) ;
#1596 = CARTESIAN_POINT ( 'NONE',  ( 7.439669587982604249, 0.9822684312230363091, 14.00000000000000000 ) ) ;
#1597 = ADVANCED_FACE ( 'NONE', ( #2851, #4174 ), #2413, .T. ) ;
#1598 = CARTESIAN_POINT ( 'NONE',  ( -8.017392084630589721, -4.988806607527435766, 13.99999999999999645 ) ) ;
#1599 = AXIS2_PLACEMENT_3D ( 'NONE', #2196, #1676, #3121 ) ;
#1600 = CARTESIAN_POINT ( 'NONE',  ( 6.034497645749724803, 4.327592090611794617, 14.00000000000000000 ) ) ;
#1601 =( GEOMETRIC_REPRESENTATION_CONTEXT ( 3 ) GLOBAL_UNCERTAINTY_ASSIGNED_CONTEXT ( ( #665 ) ) GLOBAL_UNIT_ASSIGNED_CONTEXT ( ( #5331, #4953, #1414 ) ) REPRESENTATION_CONTEXT ( 'NONE', 'WORKASPACE' ) );
#1602 = ORIENTED_EDGE ( 'NONE', *, *, #2842, .F. ) ;
#1603 = CARTESIAN_POINT ( 'NONE',  ( -3.867583043141952892, 8.914321633328466277, 1.999999999999998224 ) ) ;
#1604 = AXIS2_PLACEMENT_3D ( 'NONE', #1750, #3479, #3652 ) ;
#1605 = CYLINDRICAL_SURFACE ( 'NONE', #2246, 25.00000000000000000 ) ;
#1606 = DIRECTION ( 'NONE',  ( 1.000000000000000000, 0.000000000000000000, 0.000000000000000000 ) ) ;
#1607 = CARTESIAN_POINT ( 'NONE',  ( 1.881113203117336097, 8.098457488329447784, 1.999999999999998224 ) ) ;
#1608 = EDGE_CURVE ( 'NONE', #2874, #4349, #5402, .T. ) ;
#1609 = VECTOR ( 'NONE', #2079, 1000.000000000000000 ) ;
#1610 = STYLED_ITEM ( 'NONE', ( #4290 ), #4053 ) ;
#1611 = CARTESIAN_POINT ( 'NONE',  ( 6.000000000000000000, 0.000000000000000000, 1.999999999999998224 ) ) ;
#1612 = CARTESIAN_POINT ( 'NONE',  ( -2.965071238690786259, 6.007415411094351398, 13.99999999999999645 ) ) ;
#1613 = VECTOR ( 'NONE', #378, 999.9999999999998863 ) ;
#1614 = DIRECTION ( 'NONE',  ( 0.000000000000000000, 0.000000000000000000, 1.000000000000000000 ) ) ;
#1615 = DIRECTION ( 'NONE',  ( -0.000000000000000000, -0.000000000000000000, 1.000000000000000000 ) ) ;
#1616 = EDGE_LOOP ( 'NONE', ( #3703, #2606 ) ) ;
#1617 = AXIS2_PLACEMENT_3D ( 'NONE', #2277, #1415, #3176 ) ;
#1618 = CYLINDRICAL_SURFACE ( 'NONE', #2817, 0.2500000000000002220 ) ;
#1619 = CARTESIAN_POINT ( 'NONE',  ( 8.774740126074163982, 5.663528079765788981, 14.00000000000000000 ) ) ;
#1620 = CARTESIAN_POINT ( 'NONE',  ( -6.537688394901212341, -6.759197365500154930, 1.999999999999998224 ) ) ;
#1621 = CARTESIAN_POINT ( 'NONE',  ( 3.917689075872249571, 9.035181080458080771, 13.99999999999999645 ) ) ;
#1622 = EDGE_CURVE ( 'NONE', #1251, #1556, #1925, .T. ) ;
#1623 = CIRCLE ( 'NONE', #5571, 3.799999999999999378 ) ;
#1624 = CARTESIAN_POINT ( 'NONE',  ( 10.48651993945768623, 0.8648464362367445091, 14.00000000000000000 ) ) ;
#1625 = ORIENTED_EDGE ( 'NONE', *, *, #2209, .F. ) ;
#1626 = LINE ( 'NONE', #758, #1613 ) ;
#1627 = ORIENTED_EDGE ( 'NONE', *, *, #5109, .F. ) ;
#1628 = CARTESIAN_POINT ( 'NONE',  ( -5.000000000000000000, 4.999999999999978684, 8.000000000000000000 ) ) ;
#1629 = CARTESIAN_POINT ( 'NONE',  ( 2.672042568001582907, -6.151894458592797932, 14.00000000000000000 ) ) ;
#1630 = CARTESIAN_POINT ( 'NONE',  ( -5.432680616545222385, 3.899654942179428652, 2.000000000001176392 ) ) ;
#1631 = AXIS2_PLACEMENT_3D ( 'NONE', #2021, #3289, #1563 ) ;
#1632 = CARTESIAN_POINT ( 'NONE',  ( -3.715337444063475658, -5.771435016728993617, 14.00000000000000000 ) ) ;
#1633 = AXIS2_PLACEMENT_3D ( 'NONE', #1926, #3682, #4060 ) ;
#1634 = EDGE_LOOP ( 'NONE', ( #1374, #3177, #5626, #5423 ) ) ;
#1635 = CARTESIAN_POINT ( 'NONE',  ( -9.500632974892678106, -0.6255030753161154866, 1.999999999999998224 ) ) ;
#1636 = EDGE_CURVE ( 'NONE', #2131, #5617, #897, .T. ) ;
#1637 = AXIS2_PLACEMENT_3D ( 'NONE', #3172, #5352, #3944 ) ;
#1638 = LINE ( 'NONE', #2469, #2519 ) ;
#1639 = PRESENTATION_STYLE_ASSIGNMENT (( #3822 ) ) ;
#1640 = CARTESIAN_POINT ( 'NONE',  ( 5.648567055624510225, 4.800053419556092216, 1.999999999999998224 ) ) ;
#1641 = CYLINDRICAL_SURFACE ( 'NONE', #3656, 0.2500000000000002220 ) ;
#1642 = CARTESIAN_POINT ( 'NONE',  ( -5.745624475482375537, 5.035517847229356470, 13.99999999999999645 ) ) ;
#1643 = EDGE_CURVE ( 'NONE', #5218, #3309, #5673, .T. ) ;
#1644 = CARTESIAN_POINT ( 'NONE',  ( -5.592500163775054212, 7.275211197852026856, 1.999999999999998224 ) ) ;
#1645 = CARTESIAN_POINT ( 'NONE',  ( 1.300000000000000044, -0.7216878364870319418, 1.249999999999999778 ) ) ;
#1646 = SURFACE_STYLE_FILL_AREA ( #4776 ) ;
#1647 = ORIENTED_EDGE ( 'NONE', *, *, #1995, .F. ) ;
#1648 = LINE ( 'NONE', #4324, #4111 ) ;
#1649 = CARTESIAN_POINT ( 'NONE',  ( 1.380000000000002558, 22.95856267278071527, 5.000000000000000000 ) ) ;
#1650 = CARTESIAN_POINT ( 'NONE',  ( -5.250997584835957355, 8.145342823909338392, 13.99999999999999645 ) ) ;
#1651 = ADVANCED_BREP_SHAPE_REPRESENTATION ( '', ( #2595, #1336 ), #1859 ) ;
#1652 = CARTESIAN_POINT ( 'NONE',  ( 9.602236826902712963, 4.172718697305597857, 14.00000000000000000 ) ) ;
#1653 = ORIENTED_EDGE ( 'NONE', *, *, #2134, .F. ) ;
#1654 = DIRECTION ( 'NONE',  ( -0.000000000000000000, -0.000000000000000000, 1.000000000000000000 ) ) ;
#1655 = VERTEX_POINT ( 'NONE', #4518 ) ;
#1656 = DIRECTION ( 'NONE',  ( -1.000000000000000000, 0.000000000000000000, 0.000000000000000000 ) ) ;
#1657 = CARTESIAN_POINT ( 'NONE',  ( 5.195030181282107584, -4.117271336869512410, 14.00000000000000000 ) ) ;
#1658 = CARTESIAN_POINT ( 'NONE',  ( -6.551010013419180211, 0.8677952034721564400, 1.999999999999998224 ) ) ;
#1659 = CARTESIAN_POINT ( 'NONE',  ( 1.540339863274486465, 7.144097608501355445, 14.00000000000000000 ) ) ;
#1660 = ORIENTED_EDGE ( 'NONE', *, *, #4578, .F. ) ;
#1661 = CARTESIAN_POINT ( 'NONE',  ( -2.179108132477198367, -10.08557389312680108, 1.999999999999998224 ) ) ;
#1662 = LINE ( 'NONE', #5630, #4817 ) ;
#1663 =( NAMED_UNIT ( * ) PLANE_ANGLE_UNIT ( ) SI_UNIT ( $, .RADIAN. ) );
#1664 = CARTESIAN_POINT ( 'NONE',  ( 7.925371078819430259, 2.990572132494937474, 1.999999999999998224 ) ) ;
#1665 = CARTESIAN_POINT ( 'NONE',  ( 1.820000000000000062, 0.000000000000000000, 0.000000000000000000 ) ) ;
#1666 = CARTESIAN_POINT ( 'NONE',  ( 3.471913601335457233, 7.039518430846527508, 13.99999999999999645 ) ) ;
#1667 = EDGE_CURVE ( 'NONE', #2953, #5376, #2003, .T. ) ;
#1668 = SHAPE_REPRESENTATION_RELATIONSHIP ( 'NONE' , 'NONE' ,  #3487, #69 ) ;
#1669 = CARTESIAN_POINT ( 'NONE',  ( -4.668631340267960894, 9.078485505801564770, 1.999999999999998224 ) ) ;
#1670 = DIRECTION ( 'NONE',  ( 0.000000000000000000, 0.000000000000000000, -1.000000000000000000 ) ) ;
#1671 = CARTESIAN_POINT ( 'NONE',  ( -5.000000000000000000, 0.000000000000000000, -8.000000000000000000 ) ) ;
#1672 = ORIENTED_EDGE ( 'NONE', *, *, #2121, .F. ) ;
#1673 = DIRECTION ( 'NONE',  ( -0.000000000000000000, -0.000000000000000000, -1.000000000000000000 ) ) ;
#1674 = LINE ( 'NONE', #3889, #3633 ) ;
#1675 = CARTESIAN_POINT ( 'NONE',  ( -9.500632974893353122, -0.6255030753161997525, 13.99999999999999645 ) ) ;
#1676 = DIRECTION ( 'NONE',  ( -1.000000000000000000, 0.000000000000000000, 0.000000000000000000 ) ) ;
#1677 = ORIENTED_EDGE ( 'NONE', *, *, #5109, .T. ) ;
#1678 = DIRECTION ( 'NONE',  ( 2.891205793294678326E-16, -1.129377263005733721E-18, 1.000000000000000000 ) ) ;
#1679 = EDGE_LOOP ( 'NONE', ( #3362, #5619, #5333, #2493 ) ) ;
#1680 = CARTESIAN_POINT ( 'NONE',  ( 1.380000000000002558, 0.000000000000000000, 4.000000000000000000 ) ) ;
#1681 = CARTESIAN_POINT ( 'NONE',  ( 0.5141566911144540564, -7.748312628312728378, 14.00000000000000000 ) ) ;
#1682 = CARTESIAN_POINT ( 'NONE',  ( 4.476660083460862971, 9.887553134100658170, 13.99999999999999645 ) ) ;
#1683 = DIRECTION ( 'NONE',  ( -1.000000000000000000, 0.000000000000000000, 0.000000000000000000 ) ) ;
#1684 = CARTESIAN_POINT ( 'NONE',  ( 7.097632634466814139, -2.668286824980076855, 14.00000000000000000 ) ) ;
#1685 = ORIENTED_EDGE ( 'NONE', *, *, #4947, .F. ) ;
#1686 = CARTESIAN_POINT ( 'NONE',  ( -10.17357856257854110, 2.902115915870757679, 1.999999999999998224 ) ) ;
#1687 = CARTESIAN_POINT ( 'NONE',  ( 6.997680802075244344, 0.4609939245309428446, 13.99999999999999645 ) ) ;
#1688 = AXIS2_PLACEMENT_3D ( 'NONE', #2651, #85, #4800 ) ;
#1689 =( NAMED_UNIT ( * ) SI_UNIT ( $, .STERADIAN. ) SOLID_ANGLE_UNIT ( ) );
#1690 = CARTESIAN_POINT ( 'NONE',  ( -0.1241967792452471353, -7.777596356722545679, 1.999999999999998224 ) ) ;
#1691 = CARTESIAN_POINT ( 'NONE',  ( -6.551010013419180211, 0.8677952034721564400, 1.999999999999998224 ) ) ;
#1692 = CARTESIAN_POINT ( 'NONE',  ( -6.762100275670005267, 3.470635719505328787, 13.99999999999999645 ) ) ;
#1693 = CONICAL_SURFACE ( 'NONE', #2984, 1732.050807568856271, 1.047197551196592524 ) ;
#1694 = SHAPE_REPRESENTATION_RELATIONSHIP ( 'NONE' , 'NONE' ,  #5261, #4053 ) ;
#1695 = CARTESIAN_POINT ( 'NONE',  ( -4.983290658055095967, 7.721050520723657051, 1.999999999999998224 ) ) ;
#1696 = VECTOR ( 'NONE', #1406, 1000.000000000000000 ) ;
#1697 = EDGE_CURVE ( 'NONE', #5417, #2170, #4021, .T. ) ;
#1698 = CARTESIAN_POINT ( 'NONE',  ( 17.99999999999999289, -17.34935157289748631, 4.000000000000000000 ) ) ;
#1699 = DIRECTION ( 'NONE',  ( -1.000000000000000000, 0.000000000000000000, 0.000000000000000000 ) ) ;
#1700 = ORIENTED_EDGE ( 'NONE', *, *, #5176, .F. ) ;
#1701 = DIRECTION ( 'NONE',  ( 0.000000000000000000, 0.000000000000000000, 1.000000000000000000 ) ) ;
#1702 = FACE_OUTER_BOUND ( 'NONE', #3953, .T. ) ;
#1703 = VECTOR ( 'NONE', #5157, 1000.000000000000000 ) ;
#1704 = CARTESIAN_POINT ( 'NONE',  ( 3.158576809044846279, 9.313732666428190754, 13.99999999999999645 ) ) ;
#1705 = ADVANCED_FACE ( 'NONE', ( #5001 ), #1061, .T. ) ;
#1706 = DIRECTION ( 'NONE',  ( 0.000000000000000000, 0.000000000000000000, -1.000000000000000000 ) ) ;
#1708 = EDGE_LOOP ( 'NONE', ( #4955, #2629, #2200, #4897 ) ) ;
#1707 = AXIS2_PLACEMENT_3D ( 'NONE', #3491, #355, #2109 ) ;
#1709 = DIRECTION ( 'NONE',  ( -1.000000000000000000, 0.000000000000000000, -0.000000000000000000 ) ) ;
#1710 = ORIENTED_EDGE ( 'NONE', *, *, #319, .T. ) ;
#1711 = DIRECTION ( 'NONE',  ( 0.000000000000000000, 0.000000000000000000, -1.000000000000000000 ) ) ;
#1712 = CARTESIAN_POINT ( 'NONE',  ( 0.5385325299235224072, 8.270587056550175120, 14.00000000000000000 ) ) ;
#1713 = CARTESIAN_POINT ( 'NONE',  ( 3.426039378954556902, 5.938690629332269211, 1.999999999999998224 ) ) ;
#1714 = PRODUCT_DEFINITION_CONTEXT ( 'detailed design', #3576, 'design' ) ;
#1715 = AXIS2_PLACEMENT_3D ( 'NONE', #3287, #5416, #2018 ) ;
#1716 = EDGE_CURVE ( 'NONE', #5397, #5155, #4144, .T. ) ;
#1717 = CARTESIAN_POINT ( 'NONE',  ( 8.673617379884035472E-16, 0.000000000000000000, 0.000000000000000000 ) ) ;
#1718 = CARTESIAN_POINT ( 'NONE',  ( -5.581220830679986200, 5.949058968288507110, 14.00000000000000000 ) ) ;
#1719 = VERTEX_POINT ( 'NONE', #3282 ) ;
#1720 = CIRCLE ( 'NONE', #2081, 5.000000000000000000 ) ;
#1721 = PLANE ( 'NONE',  #5033 ) ;
#1722 = CARTESIAN_POINT ( 'NONE',  ( 1.869626052002640648, 6.555486721476421863, 13.99999999999999645 ) ) ;
#1723 = VECTOR ( 'NONE', #4700, 1000.000000000000000 ) ;
#1724 = CARTESIAN_POINT ( 'NONE',  ( -6.681386044268610824, 6.252046474378027519, 1.999999999999998224 ) ) ;
#1725 = CARTESIAN_POINT ( 'NONE',  ( 1.869626052002579808, 6.555486721476420087, 1.999999999999998224 ) ) ;
#1726 = AXIS2_PLACEMENT_3D ( 'NONE', #723, #5172, #5123 ) ;
#1727 = CARTESIAN_POINT ( 'NONE',  ( 3.747087600548785868, -7.295897990121166465, 13.99999999999999645 ) ) ;
#1728 = FACE_OUTER_BOUND ( 'NONE', #4142, .T. ) ;
#1729 = SURFACE_STYLE_USAGE ( .BOTH. , #456 ) ;
#1730 = DIRECTION ( 'NONE',  ( -1.000000000000000000, 0.000000000000000000, 0.000000000000000000 ) ) ;
#1731 = LINE ( 'NONE', #2999, #2262 ) ;
#1732 = LINE ( 'NONE', #2191, #1910 ) ;
#1733 = VERTEX_POINT ( 'NONE', #4659 ) ;
#1734 = LINE ( 'NONE', #5, #4383 ) ;
#1735 = CARTESIAN_POINT ( 'NONE',  ( -7.551678268146210016, 5.989845445213457964, 13.99999999999999645 ) ) ;
#1736 = ORIENTED_EDGE ( 'NONE', *, *, #937, .T. ) ;
#1737 = DIRECTION ( 'NONE',  ( -1.000000000000000000, -0.000000000000000000, -0.000000000000000000 ) ) ;
#1738 = EDGE_LOOP ( 'NONE', ( #3774, #739, #1068, #5199, #1051, #3753 ) ) ;
#1739 = CARTESIAN_POINT ( 'NONE',  ( -5.000000000000000000, 4.999999999999978684, 5.000000000000000000 ) ) ;
#1740 = CARTESIAN_POINT ( 'NONE',  ( -6.700137237868793783, -5.881230172876196427, 14.00000000000000000 ) ) ;
#1741 = CARTESIAN_POINT ( 'NONE',  ( -2.440069559021786905, 10.46881825416662259, 13.99999999999999645 ) ) ;
#1742 = FACE_OUTER_BOUND ( 'NONE', #1302, .T. ) ;
#1743 = CARTESIAN_POINT ( 'NONE',  ( -6.667513054348625623, -4.302816426345352774, 14.00000000000000000 ) ) ;
#1744 = ORIENTED_EDGE ( 'NONE', *, *, #1866, .F. ) ;
#1745 = DIRECTION ( 'NONE',  ( 1.000000000000000000, 4.364351673553916694E-15, 0.000000000000000000 ) ) ;
#1746 = CARTESIAN_POINT ( 'NONE',  ( 6.026041665150466464, -0.9817477132364120784, 13.99999999999999645 ) ) ;
#1747 = APPLICATION_PROTOCOL_DEFINITION ( 'draft international standard', 'automotive_design', 1998, #2071 ) ;
#1748 = CARTESIAN_POINT ( 'NONE',  ( 8.549805251451806143, -4.382211019330641832, 1.999999999999998224 ) ) ;
#1749 = CARTESIAN_POINT ( 'NONE',  ( 3.426039378954556902, 5.938690629332269211, 1.999999999999998224 ) ) ;
#1750 = CARTESIAN_POINT ( 'NONE',  ( 0.000000000000000000, 0.000000000000000000, 0.000000000000000000 ) ) ;
#1751 = PRESENTATION_STYLE_ASSIGNMENT (( #3596 ) ) ;
#1752 = CARTESIAN_POINT ( 'NONE',  ( 5.500000000000000000, 0.000000000000000000, 1.999999999999998224 ) ) ;
#1753 = CARTESIAN_POINT ( 'NONE',  ( -2.744490807750914030, 5.556819979548925481, 1.999999999999998224 ) ) ;
#1754 = DIRECTION ( 'NONE',  ( -0.000000000000000000, -0.000000000000000000, 1.000000000000000000 ) ) ;
#1755 = VERTEX_POINT ( 'NONE', #4256 ) ;
#1756 = DIRECTION ( 'NONE',  ( -0.000000000000000000, -0.000000000000000000, 1.000000000000000000 ) ) ;
#1757 = CARTESIAN_POINT ( 'NONE',  ( 10.98697916625460991, 0.8999353979983718554, 13.99999999999999645 ) ) ;
#1758 = CARTESIAN_POINT ( 'NONE',  ( 4.336808689942017736E-16, -0.7216878364870318308, 1.249999999999999778 ) ) ;
#1759 = EDGE_LOOP ( 'NONE', ( #3032, #3001 ) ) ;
#1760 = CARTESIAN_POINT ( 'NONE',  ( 0.000000000000000000, 0.000000000000000000, 4.000000000000000000 ) ) ;
#1761 = ORIENTED_EDGE ( 'NONE', *, *, #4480, .F. ) ;
#1762 = ORIENTED_EDGE ( 'NONE', *, *, #4513, .T. ) ;
#1763 = CARTESIAN_POINT ( 'NONE',  ( -3.391372024942433949, 7.476497417048839189, 14.00000000000000000 ) ) ;
#1764 = CARTESIAN_POINT ( 'NONE',  ( 6.997680802075242568, 0.4609939245310665235, 1.999999999999998224 ) ) ;
#1765 = DIRECTION ( 'NONE',  ( 0.06000000000000009492, -0.9981983770774225384, -0.000000000000000000 ) ) ;
#1766 = PRESENTATION_LAYER_ASSIGNMENT (  '', '', ( #4251 ) ) ;
#1767 = CARTESIAN_POINT ( 'NONE',  ( 7.716263785693138644, -3.801003699433110228, 14.00000000000000000 ) ) ;
#1768 = ADVANCED_FACE ( 'NONE', ( #4318 ), #1641, .T. ) ;
#1769 = ORIENTED_EDGE ( 'NONE', *, *, #3650, .T. ) ;
#1770 = CARTESIAN_POINT ( 'NONE',  ( 4.476660083460862971, 9.887553134099890784, 1.999999999999998224 ) ) ;
#1771 = LINE ( 'NONE', #3527, #533 ) ;
#1772 = AXIS2_PLACEMENT_3D ( 'NONE', #4253, #5148, #2902 ) ;
#1773 = CARTESIAN_POINT ( 'NONE',  ( 5.194219494279654015, 4.554949839096549269, 13.99999999999999645 ) ) ;
#1774 = SHAPE_DEFINITION_REPRESENTATION ( #684, #953 ) ;
#1775 = CARTESIAN_POINT ( 'NONE',  ( -0.7616497023963333390, 9.236585841460744462, 1.999999999999998224 ) ) ;
#1776 = CARTESIAN_POINT ( 'NONE',  ( 6.444084565535371567, 4.617298776321547393, 1.999999999999998224 ) ) ;
#1777 = VECTOR ( 'NONE', #869, 1000.000000000000000 ) ;
#1778 = FACE_BOUND ( 'NONE', #1634, .T. ) ;
#1779 = CARTESIAN_POINT ( 'NONE',  ( 10.48651993945612126, 0.8648464362367445091, 1.999999999999998224 ) ) ;
#1780 = EDGE_CURVE ( 'NONE', #4073, #2517, #1357, .T. ) ;
#1781 = CARTESIAN_POINT ( 'NONE',  ( 23.24999999999999645, -8.485281374238580199, -8.000000000000000000 ) ) ;
#1782 = CARTESIAN_POINT ( 'NONE',  ( 0.000000000000000000, 0.000000000000000000, 8.000000000000000000 ) ) ;
#1783 = ORIENTED_EDGE ( 'NONE', *, *, #5268, .T. ) ;
#1784 = DIRECTION ( 'NONE',  ( 0.9999273757268464236, -0.01205169166640770832, 0.000000000000000000 ) ) ;
#1785 = AXIS2_PLACEMENT_3D ( 'NONE', #597, #4169, #1921 ) ;
#1786 = CARTESIAN_POINT ( 'NONE',  ( 4.476660083460862971, 9.887553134100658170, 13.99999999999999645 ) ) ;
#1787 = CARTESIAN_POINT ( 'NONE',  ( 0.000000000000000000, 0.000000000000000000, 5.000000000000000000 ) ) ;
#1788 = DIRECTION ( 'NONE',  ( 0.000000000000000000, 0.000000000000000000, 1.000000000000000000 ) ) ;
#1789 = EDGE_LOOP ( 'NONE', ( #922, #4542, #3410, #4328 ) ) ;
#1790 = AXIS2_PLACEMENT_3D ( 'NONE', #1436, #3194, #4944 ) ;
#1791 = EDGE_LOOP ( 'NONE', ( #816, #797, #1799, #4616 ) ) ;
#1792 = COLOUR_RGB ( '',0.8941176470588234615, 0.8941176470588234615, 0.8941176470588234615 ) ;
#1793 = CARTESIAN_POINT ( 'NONE',  ( -8.757712506721391676, -2.046213373001789737, 14.00000000000000000 ) ) ;
#1794 = CARTESIAN_POINT ( 'NONE',  ( -1.189470317277863121, -7.202885406307536265, 1.999999999999998224 ) ) ;
#1795 = ADVANCED_FACE ( 'NONE', ( #3794 ), #1150, .T. ) ;
#1796 = AXIS2_PLACEMENT_3D ( 'NONE', #3149, #3516, #4496 ) ;
#1797 = DIRECTION ( 'NONE',  ( -1.000000000000000000, -0.000000000000000000, -0.000000000000000000 ) ) ;
#1798 = CARTESIAN_POINT ( 'NONE',  ( 3.520917041835319505, -6.848083076131263880, 14.00000000000000000 ) ) ;
#1799 = ORIENTED_EDGE ( 'NONE', *, *, #3717, .F. ) ;
#1800 = CARTESIAN_POINT ( 'NONE',  ( 1.176163838800080574, -10.19826953922189539, 1.999999999999998224 ) ) ;
#1801 = CARTESIAN_POINT ( 'NONE',  ( 0.000000000000000000, 0.000000000000000000, 14.00000000000000000 ) ) ;
#1802 = AXIS2_PLACEMENT_3D ( 'NONE', #5128, #1614, #5585 ) ;
#1803 = CARTESIAN_POINT ( 'NONE',  ( 6.938542625487071902, -1.260128425111980643, 13.99999999999999645 ) ) ;
#1804 = CARTESIAN_POINT ( 'NONE',  ( -8.913799778910963312, 1.613954699392611047, 1.999999999999998224 ) ) ;
#1805 = CARTESIAN_POINT ( 'NONE',  ( 1.183015137239217474, -7.150809911821259135, 1.999999999999998224 ) ) ;
#1806 = EDGE_CURVE ( 'NONE', #73, #5593, #2472, .T. ) ;
#1807 = FILL_AREA_STYLE ('',( #52 ) ) ;
#1808 = AXIS2_PLACEMENT_3D ( 'NONE', #4331, #3039, #357 ) ;
#1809 = APPLICATION_CONTEXT ( 'automotive_design' ) ;
#1810 = FACE_OUTER_BOUND ( 'NONE', #2083, .T. ) ;
#1811 = CARTESIAN_POINT ( 'NONE',  ( -0.3669926094919909731, -5.824518274481597757, 1.999999999999998224 ) ) ;
#1812 = CIRCLE ( 'NONE', #2462, 4.500000000000000888 ) ;
#1813 = CYLINDRICAL_SURFACE ( 'NONE', #1413, 23.00000000000000000 ) ;
#1814 = DIRECTION ( 'NONE',  ( -0.000000000000000000, -0.000000000000000000, -1.000000000000000000 ) ) ;
#1815 = VERTEX_POINT ( 'NONE', #4230 ) ;
#1816 = DIRECTION ( 'NONE',  ( 1.445602896647339163E-16, 0.000000000000000000, 1.000000000000000000 ) ) ;
#1817 = EDGE_CURVE ( 'NONE', #3841, #2953, #3201, .T. ) ;
#1818 = VECTOR ( 'NONE', #5687, 1000.000000000000000 ) ;
#1819 = CARTESIAN_POINT ( 'NONE',  ( -4.581738566658776435, -9.288989786611782762, 13.99999999999999645 ) ) ;
#1820 = PRESENTATION_STYLE_ASSIGNMENT (( #1904 ) ) ;
#1821 = FACE_OUTER_BOUND ( 'NONE', #443, .T. ) ;
#1822 = ORIENTED_EDGE ( 'NONE', *, *, #3881, .T. ) ;
#1823 = CARTESIAN_POINT ( 'NONE',  ( 0.000000000000000000, 0.000000000000000000, 0.000000000000000000 ) ) ;
#1824 = CARTESIAN_POINT ( 'NONE',  ( 5.071900148311402567, 7.881338450277072027, 14.00000000000000000 ) ) ;
#1825 = CARTESIAN_POINT ( 'NONE',  ( -5.810612947751084612, -4.611264106266946605, 1.999999999999998224 ) ) ;
#1826 = CARTESIAN_POINT ( 'NONE',  ( -2.138212235155099616, 7.953261502403489835, 1.999999999999998224 ) ) ;
#1827 = CARTESIAN_POINT ( 'NONE',  ( 8.618507686539667034, 3.909830026712121764, 14.00000000000000000 ) ) ;
#1828 = ORIENTED_EDGE ( 'NONE', *, *, #1211, .F. ) ;
#1829 = CARTESIAN_POINT ( 'NONE',  ( -10.48421140591450751, 1.206973991593908169, 1.999999999999998224 ) ) ;
#1830 = DIRECTION ( 'NONE',  ( 0.000000000000000000, 0.000000000000000000, 1.000000000000000000 ) ) ;
#1831 = CARTESIAN_POINT ( 'NONE',  ( -0.1462562576243747192, 8.775315755192165668, 13.99999999999999645 ) ) ;
#1832 = CARTESIAN_POINT ( 'NONE',  ( -5.745624475482375537, 5.035517847229356470, 13.99999999999999645 ) ) ;
#1833 = PRODUCT_CONTEXT ( 'NONE', #1998, 'mechanical' ) ;
#1834 = CARTESIAN_POINT ( 'NONE',  ( -8.290222237438479524, 3.747600907060152142, 1.999999999999998224 ) ) ;
#1835 = EDGE_LOOP ( 'NONE', ( #1457, #2411, #1848 ) ) ;
#1836 = CARTESIAN_POINT ( 'NONE',  ( 6.938542625487070126, -1.260128425111949557, 1.999999999999998224 ) ) ;
#1837 = CARTESIAN_POINT ( 'NONE',  ( 22.99999999999999645, -8.485281374238580199, -8.000000000000000000 ) ) ;
#1838 = DIRECTION ( 'NONE',  ( 0.000000000000000000, 0.000000000000000000, 1.000000000000000000 ) ) ;
#1839 = DIRECTION ( 'NONE',  ( -1.000000000000000000, 0.000000000000000000, 0.000000000000000000 ) ) ;
#1840 = CARTESIAN_POINT ( 'NONE',  ( 1.492118473828444536, -5.588909376072070501, 1.999999999999998224 ) ) ;
#1841 = CYLINDRICAL_SURFACE ( 'NONE', #805, 23.00000000000000000 ) ;
#1842 = EDGE_CURVE ( 'NONE', #186, #1397, #772, .T. ) ;
#1843 = DIRECTION ( 'NONE',  ( 1.000000000000000000, 0.000000000000000000, 0.000000000000000000 ) ) ;
#1844 = ADVANCED_FACE ( 'NONE', ( #2069 ), #3446, .F. ) ;
#1845 = CARTESIAN_POINT ( 'NONE',  ( 7.066195124645641812, -7.302433507960033765, 13.99999999999999645 ) ) ;
#1846 = DIRECTION ( 'NONE',  ( -0.000000000000000000, -0.000000000000000000, -1.000000000000000000 ) ) ;
#1847 = CARTESIAN_POINT ( 'NONE',  ( -1.380000000000054960, 3.291637795666119257E-15, 12.00000000000000000 ) ) ;
#1848 = ORIENTED_EDGE ( 'NONE', *, *, #81, .T. ) ;
#1849 = ORIENTED_EDGE ( 'NONE', *, *, #3485, .F. ) ;
#1850 = CARTESIAN_POINT ( 'NONE',  ( -4.668631340267771712, 9.078485505802326827, 14.00000000000000000 ) ) ;
#1851 = CARTESIAN_POINT ( 'NONE',  ( 7.812003909081975728, 1.689803927524521354, 1.999999999999998224 ) ) ;
#1852 = ADVANCED_BREP_SHAPE_REPRESENTATION ( '', ( #2585, #1336 ), #2498 ) ;
#1853 = CARTESIAN_POINT ( 'NONE',  ( -3.391372024942433505, 7.476497417048837413, 1.999999999999998224 ) ) ;
#1854 = CARTESIAN_POINT ( 'NONE',  ( -8.999716648909560135, -0.5976852874978595409, 14.00000000000000000 ) ) ;
#1855 = ORIENTED_EDGE ( 'NONE', *, *, #2354, .F. ) ;
#1856 = CARTESIAN_POINT ( 'NONE',  ( 7.775655769254118610, 6.170250810330676572, 1.999999999999998224 ) ) ;
#1857 = CARTESIAN_POINT ( 'NONE',  ( -5.000000000000000000, 0.000000000000000000, -8.000000000000000000 ) ) ;
#1858 = CARTESIAN_POINT ( 'NONE',  ( 6.401046915552173644, 6.194151307163302533, 13.99999999999999645 ) ) ;
#1859 =( GEOMETRIC_REPRESENTATION_CONTEXT ( 3 ) GLOBAL_UNCERTAINTY_ASSIGNED_CONTEXT ( ( #2115 ) ) GLOBAL_UNIT_ASSIGNED_CONTEXT ( ( #658, #225, #5030 ) ) REPRESENTATION_CONTEXT ( 'NONE', 'WORKASPACE' ) );
#1860 = CARTESIAN_POINT ( 'NONE',  ( -8.486979168634645632, -0.6954046021538184963, 13.99999999999999645 ) ) ;
#1861 = CARTESIAN_POINT ( 'NONE',  ( -8.332455577110955858, 5.761155596213678010, 1.999999999999998224 ) ) ;
#1862 = CARTESIAN_POINT ( 'NONE',  ( 5.862282306371745300, 6.688714470717011196, 1.999999999999998224 ) ) ;
#1863 = DIRECTION ( 'NONE',  ( -0.9981983770774224274, -0.06000000000000008105, 0.000000000000000000 ) ) ;
#1864 = EDGE_CURVE ( 'NONE', #525, #1594, #2993, .T. ) ;
#1865 = CARTESIAN_POINT ( 'NONE',  ( -6.069783318623453106, -0.2142533344232669390, 1.999999999999998224 ) ) ;
#1866 = EDGE_CURVE ( 'NONE', #1012, #442, #1812, .T. ) ;
#1867 = EDGE_LOOP ( 'NONE', ( #436, #3178 ) ) ;
#1868 = DIRECTION ( 'NONE',  ( -0.000000000000000000, -0.000000000000000000, -1.000000000000000000 ) ) ;
#1869 = CARTESIAN_POINT ( 'NONE',  ( -23.00000000000000000, 0.000000000000000000, -2.000000000000000000 ) ) ;
#1870 = VECTOR ( 'NONE', #3544, 1000.000000000000000 ) ;
#1871 = CARTESIAN_POINT ( 'NONE',  ( -9.913420430684192652, 3.732070475089104722, 13.99999999999999645 ) ) ;
#1872 = EDGE_CURVE ( 'NONE', #5155, #4844, #3934, .T. ) ;
#1873 = VECTOR ( 'NONE', #3100, 1000.000000000000000 ) ;
#1874 = FACE_OUTER_BOUND ( 'NONE', #2278, .T. ) ;
#1875 = DIRECTION ( 'NONE',  ( -1.000000000000000000, 0.000000000000000000, 0.000000000000000000 ) ) ;
#1876 = ORIENTED_EDGE ( 'NONE', *, *, #951, .T. ) ;
#1877 = EDGE_LOOP ( 'NONE', ( #2752, #4571, #2770, #44 ) ) ;
#1878 = CARTESIAN_POINT ( 'NONE',  ( -8.913799778910966864, 1.613954699392568859, 14.00000000000000000 ) ) ;
#1879 = CARTESIAN_POINT ( 'NONE',  ( 1.649120185255090298, 7.633850905136056575, 1.999999999999998224 ) ) ;
#1880 = VECTOR ( 'NONE', #4426, 1000.000000000000000 ) ;
#1881 = CARTESIAN_POINT ( 'NONE',  ( 8.156937663705429387, 2.333191796391003603, 1.999999999999998224 ) ) ;
#1882 = CARTESIAN_POINT ( 'NONE',  ( -0.7616497023963333390, 9.236585841461440793, 14.00000000000000000 ) ) ;
#1883 = AXIS2_PLACEMENT_3D ( 'NONE', #3941, #2586, #4886 ) ;
#1884 = ORIENTED_EDGE ( 'NONE', *, *, #1177, .F. ) ;
#1885 = CARTESIAN_POINT ( 'NONE',  ( 1.933011552319068960, 10.64041406927699640, 1.999999999999998224 ) ) ;
#1886 = CARTESIAN_POINT ( 'NONE',  ( 1.492118473828444536, -5.588909376072072277, 14.00000000000000000 ) ) ;
#1887 = CARTESIAN_POINT ( 'NONE',  ( 5.857810772706378621, -5.665644577056677456, 13.99999999999999645 ) ) ;
#1888 = EDGE_CURVE ( 'NONE', #3442, #660, #1095, .T. ) ;
#1889 = AXIS2_PLACEMENT_3D ( 'NONE', #4666, #728, #5559 ) ;
#1890 = CARTESIAN_POINT ( 'NONE',  ( 0.7175617537426050019, 6.248173425771539335, 14.00000000000000000 ) ) ;
#1891 = ORIENTED_EDGE ( 'NONE', *, *, #5677, .T. ) ;
#1892 = AXIS2_PLACEMENT_3D ( 'NONE', #1075, #1593, #270 ) ;
#1893 = CARTESIAN_POINT ( 'NONE',  ( 7.565999024956892249, -2.848076369834589450, 1.999999999999998224 ) ) ;
#1894 = CARTESIAN_POINT ( 'NONE',  ( 0.000000000000000000, 0.000000000000000000, 1.999999999999999112 ) ) ;
#1895 = AXIS2_PLACEMENT_3D ( 'NONE', #1905, #4149, #1930 ) ;
#1896 = CARTESIAN_POINT ( 'NONE',  ( -7.019001384594680815, 0.4577903460188660345, 1.999999999999998224 ) ) ;
#1897 = ORIENTED_EDGE ( 'NONE', *, *, #4420, .T. ) ;
#1898 = CARTESIAN_POINT ( 'NONE',  ( 6.034497645749723027, 4.327592090611793729, 1.999999999999998224 ) ) ;
#1899 = DIRECTION ( 'NONE',  ( 1.000000000000000000, 0.000000000000000000, 0.000000000000000000 ) ) ;
#1900 = CIRCLE ( 'NONE', #1170, 3.799999999999999378 ) ;
#1901 = CARTESIAN_POINT ( 'NONE',  ( 22.00000000000000000, 0.000000000000000000, 12.00000000000000000 ) ) ;
#1902 = CARTESIAN_POINT ( 'NONE',  ( -12.50000000000000000, 0.000000000000000000, 14.00000000000000000 ) ) ;
#1903 = AXIS2_PLACEMENT_3D ( 'NONE', #5424, #160, #1571 ) ;
#1904 = SURFACE_STYLE_USAGE ( .BOTH. , #90 ) ;
#1905 = CARTESIAN_POINT ( 'NONE',  ( 10.20000000000000107, 0.000000000000000000, 0.000000000000000000 ) ) ;
#1906 = EDGE_LOOP ( 'NONE', ( #4564, #3540, #1647, #2028, #971, #2722 ) ) ;
#1907 = CARTESIAN_POINT ( 'NONE',  ( 0.000000000000000000, 0.000000000000000000, 8.000000000000000000 ) ) ;
#1908 = CARTESIAN_POINT ( 'NONE',  ( -2.331745755519268215, 9.978964459600446091, 14.00000000000000000 ) ) ;
#1909 = CARTESIAN_POINT ( 'NONE',  ( -3.441860715206332078, -7.602597312514155270, 1.999999999999998224 ) ) ;
#1910 = VECTOR ( 'NONE', #2243, 1000.000000000000000 ) ;
#1911 = SHAPE_REPRESENTATION ( 'tape', ( #1336 ), #5538 ) ;
#1912 = CARTESIAN_POINT ( 'NONE',  ( 6.037635170864973588, 5.848285684830694997, 1.999999999999998224 ) ) ;
#1913 = CARTESIAN_POINT ( 'NONE',  ( 8.256732931686221022, 4.597988481711512421, 14.00000000000000000 ) ) ;
#1914 = EDGE_LOOP ( 'NONE', ( #5160, #1991, #895, #440 ) ) ;
#1915 = LINE ( 'NONE', #3238, #2823 ) ;
#1916 = CARTESIAN_POINT ( 'NONE',  ( 0.000000000000000000, -0.7216878364870318308, 1.249999999999999778 ) ) ;
#1917 = CARTESIAN_POINT ( 'NONE',  ( -8.126042061586270293, 2.755650963504471473, 13.99999999999999645 ) ) ;
#1918 = CARTESIAN_POINT ( 'NONE',  ( -2.331745755519268215, 9.978964459600444314, 1.999999999999998224 ) ) ;
#1919 = ORIENTED_EDGE ( 'NONE', *, *, #1643, .F. ) ;
#1920 = CARTESIAN_POINT ( 'NONE',  ( 1.954797901281672967, -9.037865403626939909, 1.999999999999998224 ) ) ;
#1921 = DIRECTION ( 'NONE',  ( 0.000000000000000000, 0.000000000000000000, 1.000000000000000000 ) ) ;
#1922 = CARTESIAN_POINT ( 'NONE',  ( -4.975175822334872322, 5.137265612443480123, 1.999999999999998224 ) ) ;
#1923 = ORIENTED_EDGE ( 'NONE', *, *, #4062, .T. ) ;
#1924 = CARTESIAN_POINT ( 'NONE',  ( 2.690160903457118557, 6.823041841979407884, 1.999999999999998224 ) ) ;
#1925 = LINE ( 'NONE', #1442, #529 ) ;
#1926 = CARTESIAN_POINT ( 'NONE',  ( 2.200000000000000178, 0.000000000000000000, 0.000000000000000000 ) ) ;
#1927 = EDGE_CURVE ( 'NONE', #3499, #4270, #5628, .T. ) ;
#1928 = DIRECTION ( 'NONE',  ( 0.000000000000000000, 0.000000000000000000, -1.000000000000000000 ) ) ;
#1929 = FILL_AREA_STYLE ('',( #62 ) ) ;
#1930 = DIRECTION ( 'NONE',  ( 0.000000000000000000, 0.000000000000000000, 1.000000000000000000 ) ) ;
#1931 = VERTEX_POINT ( 'NONE', #2208 ) ;
#1932 = DIRECTION ( 'NONE',  ( 0.000000000000000000, 0.000000000000000000, 1.000000000000000000 ) ) ;
#1933 = CARTESIAN_POINT ( 'NONE',  ( -3.672794075660814617, 8.451992513476522362, 14.00000000000000000 ) ) ;
#1934 = CARTESIAN_POINT ( 'NONE',  ( 8.396466517619506575, 3.163083589105210258, 1.999999999999998224 ) ) ;
#1935 = ADVANCED_FACE ( 'NONE', ( #4419 ), #1721, .F. ) ;
#1936 = CARTESIAN_POINT ( 'NONE',  ( 1.881113203117336097, 8.098457488329447784, 1.999999999999998224 ) ) ;
#1937 = CARTESIAN_POINT ( 'NONE',  ( 0.3244988297792451570, -9.772062696132405080, 14.00000000000000000 ) ) ;
#1938 = DIRECTION ( 'NONE',  ( 0.000000000000000000, 0.000000000000000000, 1.000000000000000000 ) ) ;
#1939 = ORIENTED_EDGE ( 'NONE', *, *, #3806, .T. ) ;
#1940 = CARTESIAN_POINT ( 'NONE',  ( 0.000000000000000000, 1.443375672974065216, 7.017607234860990640E-28 ) ) ;
#1941 = CARTESIAN_POINT ( 'NONE',  ( 4.815977876496241095, 4.225366587634054483, 14.00000000000000000 ) ) ;
#1942 = CARTESIAN_POINT ( 'NONE',  ( 10.02932042447482353, 0.1670047327946668492, 13.99999999999999645 ) ) ;
#1943 = ADVANCED_FACE ( 'NONE', ( #388 ), #4880, .T. ) ;
#1944 = CARTESIAN_POINT ( 'NONE',  ( 10.50003631213657762, 0.006025845833179020727, 1.999999999999998224 ) ) ;
#1945 = ORIENTED_EDGE ( 'NONE', *, *, #2908, .F. ) ;
#1946 = CARTESIAN_POINT ( 'NONE',  ( 7.761517335261689965, -2.213789340049559407, 1.999999999999998224 ) ) ;
#1947 = DIRECTION ( 'NONE',  ( -0.000000000000000000, -0.000000000000000000, 1.000000000000000000 ) ) ;
#1948 = CARTESIAN_POINT ( 'NONE',  ( -0.2403693791186040096, 7.265099133626553574, 1.999999999999998224 ) ) ;
#1949 = MECHANICAL_DESIGN_GEOMETRIC_PRESENTATION_REPRESENTATION (  '', ( #477 ), #211 ) ;
#1950 = VERTEX_POINT ( 'NONE', #19 ) ;
#1951 = CARTESIAN_POINT ( 'NONE',  ( 7.494325059173603698, -0.8592991332473469690, 1.999999999999998224 ) ) ;
#1952 = CARTESIAN_POINT ( 'NONE',  ( 23.00000000000000000, -2.168404344971008868E-16, 8.000000000000000000 ) ) ;
#1953 = SURFACE_STYLE_FILL_AREA ( #3204 ) ;
#1954 = ADVANCED_FACE ( 'NONE', ( #5659, #3474 ), #936, .F. ) ;
#1955 = DIRECTION ( 'NONE',  ( -0.000000000000000000, -0.000000000000000000, 1.000000000000000000 ) ) ;
#1956 = PLANE ( 'NONE',  #4814 ) ;
#1957 = CARTESIAN_POINT ( 'NONE',  ( 1.500000000000002887, 24.95495942693556657, 5.000000000000000000 ) ) ;
#1958 = EDGE_LOOP ( 'NONE', ( #4056, #387, #2428, #1215 ) ) ;
#1959 = FACE_OUTER_BOUND ( 'NONE', #3118, .T. ) ;
#1960 = LINE ( 'NONE', #541, #505 ) ;
#1961 = CARTESIAN_POINT ( 'NONE',  ( 9.020117466466054168, 0.2947087185667776055, 1.999999999999998224 ) ) ;
#1962 = CARTESIAN_POINT ( 'NONE',  ( 6.033242055734853615, 5.122103984031451063, 13.99999999999999645 ) ) ;
#1963 = CARTESIAN_POINT ( 'NONE',  ( 1.837295235934470305, 10.14794156482770049, 1.999999999999998224 ) ) ;
#1964 = DIRECTION ( 'NONE',  ( 1.000000000000000000, 0.000000000000000000, 0.000000000000000000 ) ) ;
#1965 = EDGE_LOOP ( 'NONE', ( #5434, #2059, #2085, #4112, #786 ) ) ;
#1966 = PRODUCT_DEFINITION_SHAPE ( 'NONE', 'NONE',  #3839 ) ;
#1967 = DIRECTION ( 'NONE',  ( -0.000000000000000000, -0.000000000000000000, 1.000000000000000000 ) ) ;
#1968 = ORIENTED_EDGE ( 'NONE', *, *, #1510, .F. ) ;
#1969 = DIRECTION ( 'NONE',  ( 0.000000000000000000, 0.000000000000000000, 1.000000000000000000 ) ) ;
#1970 = CIRCLE ( 'NONE', #4719, 2.000000000000000000 ) ;
#1971 = CARTESIAN_POINT ( 'NONE',  ( -2.189112655477411185, -6.464091385745795115, 14.00000000000000000 ) ) ;
#1972 = CARTESIAN_POINT ( 'NONE',  ( -7.044187934146358465, 6.598551529630926282, 13.99999999999999645 ) ) ;
#1973 = EDGE_CURVE ( 'NONE', #2459, #2880, #5495, .T. ) ;
#1974 = AXIS2_PLACEMENT_3D ( 'NONE', #1383, #4375, #4828 ) ;
#1975 = CARTESIAN_POINT ( 'NONE',  ( -6.398096652174580790, -7.548242073784104278, 1.999999999999998224 ) ) ;
#1976 = ORIENTED_EDGE ( 'NONE', *, *, #4934, .T. ) ;
#1977 = CARTESIAN_POINT ( 'NONE',  ( -3.441860715206332078, -7.602597312514155270, 1.999999999999998224 ) ) ;
#1978 = AXIS2_PLACEMENT_3D ( 'NONE', #4237, #1564, #288 ) ;
#1979 = CARTESIAN_POINT ( 'NONE',  ( 17.74999999999999289, -15.01665741768121443, -8.000000000000000000 ) ) ;
#1980 = CARTESIAN_POINT ( 'NONE',  ( -4.184906021401388898, -5.457255036755482180, 1.999999999999998224 ) ) ;
#1981 = VECTOR ( 'NONE', #3298, 1000.000000000000000 ) ;
#1982 = EDGE_CURVE ( 'NONE', #118, #4473, #4572, .T. ) ;
#1983 = VERTEX_POINT ( 'NONE', #3960 ) ;
#1984 = CARTESIAN_POINT ( 'NONE',  ( 6.445330636073144603, -1.168293168414208827, 1.999999999999998224 ) ) ;
#1985 = DIRECTION ( 'NONE',  ( 1.000000000000000000, 0.000000000000000000, 0.000000000000000000 ) ) ;
#1986 = CARTESIAN_POINT ( 'NONE',  ( -1.379999999999999893, 22.95856267278071172, 15.94994774640597512 ) ) ;
#1987 = AXIS2_PLACEMENT_3D ( 'NONE', #4347, #4489, #3509 ) ;
#1988 = UNCERTAINTY_MEASURE_WITH_UNIT (LENGTH_MEASURE( 1.000000000000000082E-05 ), #3797, 'distance_accuracy_value', 'NONE');
#1989 = AXIS2_PLACEMENT_3D ( 'NONE', #2163, #1188, #1275 ) ;
#1990 = CARTESIAN_POINT ( 'NONE',  ( 0.000000000000000000, 0.000000000000000000, 8.000000000000000000 ) ) ;
#1991 = ORIENTED_EDGE ( 'NONE', *, *, #3567, .T. ) ;
#1992 = DIRECTION ( 'NONE',  ( 1.000000000000000000, 0.000000000000000000, 0.000000000000000000 ) ) ;
#1993 = DIRECTION ( 'NONE',  ( 0.000000000000000000, -1.000000000000000000, 0.000000000000000000 ) ) ;
#1994 = CARTESIAN_POINT ( 'NONE',  ( -8.026550172065139321, -2.724140490265046122, 1.999999999999998224 ) ) ;
#1995 = EDGE_CURVE ( 'NONE', #5065, #4764, #1771, .T. ) ;
#1996 = CIRCLE ( 'NONE', #802, 0.2000000000000000944 ) ;
#1997 = CARTESIAN_POINT ( 'NONE',  ( -5.390757458300978300, 6.793134358447313836, 13.99999999999999645 ) ) ;
#1998 = APPLICATION_CONTEXT ( 'automotive_design' ) ;
#1999 = CARTESIAN_POINT ( 'NONE',  ( -4.999999999999999112, 24.49489742783178770, 24.08672805191341482 ) ) ;
#2000 = EDGE_LOOP ( 'NONE', ( #4635, #4038 ) ) ;
#2001 = CARTESIAN_POINT ( 'NONE',  ( 4.999999999999923617, 22.44994432064366308, -5.000000000000000000 ) ) ;
#2002 = VERTEX_POINT ( 'NONE', #3558 ) ;
#2003 = CIRCLE ( 'NONE', #2091, 3.799999999999999378 ) ;
#2004 = DIRECTION ( 'NONE',  ( 0.000000000000000000, 0.000000000000000000, 1.000000000000000000 ) ) ;
#2005 = CARTESIAN_POINT ( 'NONE',  ( 4.290186206382709422, 5.996800006796702220, 14.00000000000000000 ) ) ;
#2006 = CARTESIAN_POINT ( 'NONE',  ( 5.348203032363755050, 8.300083771889282147, 13.99999999999999645 ) ) ;
#2007 = CARTESIAN_POINT ( 'NONE',  ( -2.717942380035140992, -6.274577315194989957, 14.00000000000000000 ) ) ;
#2008 = ADVANCED_FACE ( 'NONE', ( #4447 ), #3021, .F. ) ;
#2009 = VERTEX_POINT ( 'NONE', #881 ) ;
#2010 = CARTESIAN_POINT ( 'NONE',  ( -8.402144917908874078, 4.670158400850170644, 1.999999999999998224 ) ) ;
#2011 = CARTESIAN_POINT ( 'NONE',  ( 23.00000000000000000, -2.168404344971008868E-16, 8.000000000000000000 ) ) ;
#2012 = CARTESIAN_POINT ( 'NONE',  ( -7.945923533235636604, 1.308497053349305439, 1.999999999999998224 ) ) ;
#2013 = ORIENTED_EDGE ( 'NONE', *, *, #4, .T. ) ;
#2014 = CARTESIAN_POINT ( 'NONE',  ( -6.334648143026943679, -2.872559841353752308, 1.999999999999998224 ) ) ;
#2015 = CARTESIAN_POINT ( 'NONE',  ( -1.424809953814531127, 6.586142414399820844, 1.999999999999998224 ) ) ;
#2016 = CARTESIAN_POINT ( 'NONE',  ( 2.321214644803172522, -6.838859567843808662, 13.99999999999999645 ) ) ;
#2017 = EDGE_CURVE ( 'NONE', #2140, #4992, #4026, .T. ) ;
#2018 = DIRECTION ( 'NONE',  ( 1.000000000000000000, 0.000000000000000000, 0.000000000000000000 ) ) ;
#2019 = CARTESIAN_POINT ( 'NONE',  ( 0.000000000000000000, 0.000000000000000000, 8.000000000000000000 ) ) ;
#2020 = ORIENTED_EDGE ( 'NONE', *, *, #267, .F. ) ;
#2021 = CARTESIAN_POINT ( 'NONE',  ( 0.000000000000000000, 0.000000000000000000, 0.000000000000000000 ) ) ;
#2022 = CARTESIAN_POINT ( 'NONE',  ( 10.48651993945768623, 0.8648464362367445091, 14.00000000000000000 ) ) ;
#2023 = CARTESIAN_POINT ( 'NONE',  ( 4.326322805049506393, -6.952463250691141461, 1.999999999999998224 ) ) ;
#2024 = CARTESIAN_POINT ( 'NONE',  ( -6.465640026559317022, 4.020973141382162552, 13.99999999999999645 ) ) ;
#2025 = CARTESIAN_POINT ( 'NONE',  ( 4.999999999999914735, 24.49489742783179835, 8.000000000000000000 ) ) ;
#2026 = ORIENTED_EDGE ( 'NONE', *, *, #1817, .F. ) ;
#2027 = CARTESIAN_POINT ( 'NONE',  ( 0.000000000000000000, 0.7216878364870328300, -1.250000000000000000 ) ) ;
#2028 = ORIENTED_EDGE ( 'NONE', *, *, #5146, .F. ) ;
#2029 = FACE_OUTER_BOUND ( 'NONE', #5048, .T. ) ;
#2030 = CARTESIAN_POINT ( 'NONE',  ( -0.8347742375825083494, 7.207659102801796891, 14.00000000000000000 ) ) ;
#2031 = CARTESIAN_POINT ( 'NONE',  ( 7.066195124645641812, -7.302433507960033765, 13.99999999999999645 ) ) ;
#2032 = EDGE_CURVE ( 'NONE', #403, #5536, #4075, .T. ) ;
#2033 = CARTESIAN_POINT ( 'NONE',  ( 6.315449825284095375, 1.474116854620425299, 14.00000000000000000 ) ) ;
#2034 = VERTEX_POINT ( 'NONE', #1427 ) ;
#2035 = CARTESIAN_POINT ( 'NONE',  ( 5.348203032363056053, 8.300083771889280371, 1.999999999999998224 ) ) ;
#2036 = CARTESIAN_POINT ( 'NONE',  ( 0.000000000000000000, 0.000000000000000000, 12.00000000000000000 ) ) ;
#2037 = CARTESIAN_POINT ( 'NONE',  ( -0.1423371034015438186, 8.273642750285960190, 1.999999999999998224 ) ) ;
#2038 = DIRECTION ( 'NONE',  ( 1.000000000000000000, 0.000000000000000000, 0.000000000000000000 ) ) ;
#2039 = CARTESIAN_POINT ( 'NONE',  ( -6.792624376349764681, -3.077375260545992752, 13.99999999999999645 ) ) ;
#2040 = PRODUCT_DEFINITION ( 'UNKNOWN', '', #2144, #384 ) ;
#2041 = DIRECTION ( 'NONE',  ( -0.7071067811865492381, 0.000000000000000000, 0.7071067811865457964 ) ) ;
#2042 = CARTESIAN_POINT ( 'NONE',  ( 2.000000000000000000, 0.000000000000000000, 8.000000000000000000 ) ) ;
#2043 = ORIENTED_EDGE ( 'NONE', *, *, #530, .T. ) ;
#2044 = CARTESIAN_POINT ( 'NONE',  ( -4.500000000000000888, 5.510910596163089556E-16, 0.000000000000000000 ) ) ;
#2045 = AXIS2_PLACEMENT_3D ( 'NONE', #4707, #2930, #770 ) ;
#2046 = CARTESIAN_POINT ( 'NONE',  ( 1.837295235934470528, 10.14794156482770404, 14.00000000000000000 ) ) ;
#2047 = CARTESIAN_POINT ( 'NONE',  ( -8.411612136543093143, -4.319922787977411360, 1.999999999999998224 ) ) ;
#2048 = CARTESIAN_POINT ( 'NONE',  ( 7.344045208303976224, 5.086154276871550195, 13.99999999999999645 ) ) ;
#2049 = CARTESIAN_POINT ( 'NONE',  ( -3.139313036748870189, 9.741172307225710369, 14.00000000000000000 ) ) ;
#2050 = ORIENTED_EDGE ( 'NONE', *, *, #2603, .T. ) ;
#2051 = CARTESIAN_POINT ( 'NONE',  ( 1.300000000000000044, -0.7216878364870318308, -1.250000000000000000 ) ) ;
#2052 = ORIENTED_EDGE ( 'NONE', *, *, #4011, .T. ) ;
#2053 = CARTESIAN_POINT ( 'NONE',  ( 0.000000000000000000, 0.000000000000000000, 4.000000000000000000 ) ) ;
#2054 = CARTESIAN_POINT ( 'NONE',  ( 6.941605245898609056, 2.746080019685927187, 14.00000000000000000 ) ) ;
#2055 = CARTESIAN_POINT ( 'NONE',  ( 3.158576809044846279, 9.313732666428190754, 13.99999999999999645 ) ) ;
#2056 = COLOUR_RGB ( '',0.8941176470588234615, 0.8941176470588234615, 0.8941176470588234615 ) ;
#2057 = CARTESIAN_POINT ( 'NONE',  ( 0.5542950790998155686, -6.736796398737816105, 14.00000000000000000 ) ) ;
#2058 = AXIS2_PLACEMENT_3D ( 'NONE', #2680, #4895, #1033 ) ;
#2059 = ORIENTED_EDGE ( 'NONE', *, *, #517, .T. ) ;
#2060 = CARTESIAN_POINT ( 'NONE',  ( -6.537688394901212341, -6.759197365500154930, 1.999999999999998224 ) ) ;
#2061 = ADVANCED_FACE ( 'NONE', ( #3614 ), #5370, .T. ) ;
#2062 = PRODUCT ( 'socket button head screw_iso_ISO 7380 - M4 x 8 - 8N', 'socket button head screw_iso_ISO 7380 - M4 x 8 - 8N', '', ( #3024 ) ) ;
#2063 = VECTOR ( 'NONE', #4115, 1000.000000000000227 ) ;
#2064 = DIRECTION ( 'NONE',  ( 0.000000000000000000, 0.000000000000000000, -1.000000000000000000 ) ) ;
#2065 = DIRECTION ( 'NONE',  ( 0.000000000000000000, 0.000000000000000000, 1.000000000000000000 ) ) ;
#2066 = CARTESIAN_POINT ( 'NONE',  ( 2.690160903457118557, 6.823041841979407884, 1.999999999999998224 ) ) ;
#2067 = VECTOR ( 'NONE', #2237, 1000.000000000000000 ) ;
#2068 = AXIS2_PLACEMENT_3D ( 'NONE', #3708, #4178, #697 ) ;
#2069 = FACE_OUTER_BOUND ( 'NONE', #3434, .T. ) ;
#2070 = CARTESIAN_POINT ( 'NONE',  ( -7.521311085815508335, -0.1255077825093697530, 13.99999999999999645 ) ) ;
#2071 = APPLICATION_CONTEXT ( 'automotive_design' ) ;
#2072 = SURFACE_STYLE_USAGE ( .BOTH. , #2963 ) ;
#2073 = CARTESIAN_POINT ( 'NONE',  ( 5.710084532570392390, 7.448680193042510389, 1.999999999999998224 ) ) ;
#2074 = FACE_OUTER_BOUND ( 'NONE', #1835, .T. ) ;
#2075 = CARTESIAN_POINT ( 'NONE',  ( 2.021687836487040535, 2.655529440325959183E-32, -2.168404344971008868E-16 ) ) ;
#2076 = ORIENTED_EDGE ( 'NONE', *, *, #1220, .T. ) ;
#2077 = AXIS2_PLACEMENT_3D ( 'NONE', #5177, #5670, #5555 ) ;
#2078 = DIRECTION ( 'NONE',  ( -0.000000000000000000, -0.000000000000000000, 1.000000000000000000 ) ) ;
#2079 = DIRECTION ( 'NONE',  ( -0.000000000000000000, -1.000000000000000000, -0.000000000000000000 ) ) ;
#2080 = CARTESIAN_POINT ( 'NONE',  ( 4.074896204546096357, -8.256886768010264888, 13.99999999999999645 ) ) ;
#2081 = AXIS2_PLACEMENT_3D ( 'NONE', #4491, #4892, #1843 ) ;
#2082 = DIRECTION ( 'NONE',  ( 1.000000000000000000, 0.000000000000000000, 0.000000000000000000 ) ) ;
#2083 = EDGE_LOOP ( 'NONE', ( #2944, #734, #5367, #4678, #818, #901, #1855 ) ) ;
#2084 = CARTESIAN_POINT ( 'NONE',  ( 0.000000000000000000, 0.000000000000000000, 12.00000000000000000 ) ) ;
#2085 = ORIENTED_EDGE ( 'NONE', *, *, #319, .F. ) ;
#2086 = CARTESIAN_POINT ( 'NONE',  ( 21.99999999999999645, -30.00000000000000000, 4.000000000000001776 ) ) ;
#2087 = CARTESIAN_POINT ( 'NONE',  ( 1.103627080440590547, -6.655442145117441477, 14.00000000000000000 ) ) ;
#2088 = CARTESIAN_POINT ( 'NONE',  ( 5.806279480217827249, -1.975834710110474512, 1.999999999999998224 ) ) ;
#2089 = CIRCLE ( 'NONE', #3556, 13.00000000000000178 ) ;
#2090 = CARTESIAN_POINT ( 'NONE',  ( 3.622712361020366867, 5.236663886535375845, 14.00000000000000000 ) ) ;
#2091 = AXIS2_PLACEMENT_3D ( 'NONE', #4545, #604, #5497 ) ;
#2092 = ORIENTED_EDGE ( 'NONE', *, *, #1927, .F. ) ;
#2093 = CARTESIAN_POINT ( 'NONE',  ( -0.7976699882155984245, 9.736979168371712845, 1.999999999999998224 ) ) ;
#2094 = DIRECTION ( 'NONE',  ( -1.000000000000000000, 0.000000000000000000, 0.000000000000000000 ) ) ;
#2095 = CARTESIAN_POINT ( 'NONE',  ( -7.550296695603107899, -2.566425989403007257, 1.999999999999998224 ) ) ;
#2096 = CARTESIAN_POINT ( 'NONE',  ( 4.999999999999923617, 22.44994432064366308, 8.000000000000000000 ) ) ;
#2097 = CARTESIAN_POINT ( 'NONE',  ( -4.492165532403490147, -5.853844512260857336, 13.99999999999999645 ) ) ;
#2098 =( NAMED_UNIT ( * ) PLANE_ANGLE_UNIT ( ) SI_UNIT ( $, .RADIAN. ) );
#2099 = CARTESIAN_POINT ( 'NONE',  ( -9.926332099420363875, -1.311590842189569894, 1.999999999999998224 ) ) ;
#2100 = CARTESIAN_POINT ( 'NONE',  ( -2.000000000000000000, 2.449293598294706414E-16, 8.000000000000000000 ) ) ;
#2101 = CARTESIAN_POINT ( 'NONE',  ( 1.300000000000000044, -0.7216878364870319418, 1.249999999999999778 ) ) ;
#2102 = APPLICATION_CONTEXT ( 'automotive_design' ) ;
#2103 = ORIENTED_EDGE ( 'NONE', *, *, #167, .F. ) ;
#2104 = CYLINDRICAL_SURFACE ( 'NONE', #4741, 5.000000000000000000 ) ;
#2105 = LINE ( 'NONE', #1837, #3908 ) ;
#2106 = CARTESIAN_POINT ( 'NONE',  ( -9.247353065532886163, -2.155497948345618919, 13.99999999999999645 ) ) ;
#2107 = DIRECTION ( 'NONE',  ( 1.000000000000000000, 0.000000000000000000, 0.000000000000000000 ) ) ;
#2108 = ORIENTED_EDGE ( 'NONE', *, *, #3321, .T. ) ;
#2109 = DIRECTION ( 'NONE',  ( 1.000000000000000000, 0.000000000000000000, 0.000000000000000000 ) ) ;
#2110 = EDGE_LOOP ( 'NONE', ( #466, #3095, #3192, #3945, #1876, #648 ) ) ;
#2111 = DIRECTION ( 'NONE',  ( 0.000000000000000000, -1.000000000000000000, 0.000000000000000000 ) ) ;
#2112 = CARTESIAN_POINT ( 'NONE',  ( 8.370269057508139099, -1.803949267857856142, 14.00000000000000000 ) ) ;
#2113 = CARTESIAN_POINT ( 'NONE',  ( -9.913420430684192652, 3.732070475089104722, 13.99999999999999645 ) ) ;
#2114 = EDGE_CURVE ( 'NONE', #1462, #1931, #345, .T. ) ;
#2115 = UNCERTAINTY_MEASURE_WITH_UNIT (LENGTH_MEASURE( 1.000000000000000082E-05 ), #658, 'distance_accuracy_value', 'NONE');
#2116 = FACE_OUTER_BOUND ( 'NONE', #1914, .T. ) ;
#2117 = CARTESIAN_POINT ( 'NONE',  ( 6.004028658818958419, -2.715480180205860794, 14.00000000000000000 ) ) ;
#2118 = EDGE_CURVE ( 'NONE', #4467, #4410, #4907, .T. ) ;
#2119 = EDGE_LOOP ( 'NONE', ( #2510, #239, #3392, #1112 ) ) ;
#2120 = CARTESIAN_POINT ( 'NONE',  ( 1.933011552319068960, 10.64041406927699640, 1.999999999999998224 ) ) ;
#2121 = EDGE_CURVE ( 'NONE', #841, #1496, #3215, .T. ) ;
#2122 = CARTESIAN_POINT ( 'NONE',  ( 6.638644669766899931, 2.135480210976827831, 13.99999999999999645 ) ) ;
#2123 = DIRECTION ( 'NONE',  ( 0.000000000000000000, 0.000000000000000000, 1.000000000000000000 ) ) ;
#2124 = CARTESIAN_POINT ( 'NONE',  ( -4.895455514773497718, -6.178604150901914061, 1.999999999999998224 ) ) ;
#2125 = DIRECTION ( 'NONE',  ( -1.000000000000000000, 0.000000000000000000, 0.000000000000000000 ) ) ;
#2126 = CARTESIAN_POINT ( 'NONE',  ( -5.402835942920536816, -5.063607225391134392, 13.99999999999999645 ) ) ;
#2127 = EDGE_CURVE ( 'NONE', #1028, #1012, #2314, .T. ) ;
#2128 = CARTESIAN_POINT ( 'NONE',  ( 2.678407690932628871, -9.362678857629568085, 1.999999999999998224 ) ) ;
#2129 = DIRECTION ( 'NONE',  ( 1.000000000000000000, 0.000000000000000000, 0.000000000000000000 ) ) ;
#2130 = PLANE ( 'NONE',  #696 ) ;
#2131 = VERTEX_POINT ( 'NONE', #3270 ) ;
#2132 = CARTESIAN_POINT ( 'NONE',  ( 0.000000000000000000, 0.000000000000000000, -8.000000000000000000 ) ) ;
#2133 = CARTESIAN_POINT ( 'NONE',  ( -5.000000000000000000, 0.000000000000000000, 8.000000000000000000 ) ) ;
#2134 = EDGE_CURVE ( 'NONE', #4643, #4872, #1078, .T. ) ;
#2135 = PRESENTATION_LAYER_ASSIGNMENT (  '', '', ( #4977 ) ) ;
#2136 = CARTESIAN_POINT ( 'NONE',  ( 0.7976699882155482424, 9.763020831628288931, 13.99999999999999645 ) ) ;
#2137 = FACE_OUTER_BOUND ( 'NONE', #214, .T. ) ;
#2138 = ORIENTED_EDGE ( 'NONE', *, *, #3394, .T. ) ;
#2139 = FACE_OUTER_BOUND ( 'NONE', #2563, .T. ) ;
#2140 = VERTEX_POINT ( 'NONE', #1857 ) ;
#2141 = CARTESIAN_POINT ( 'NONE',  ( 2.400000000000000799, 0.000000000000000000, 2.199999999999999289 ) ) ;
#2142 = CARTESIAN_POINT ( 'NONE',  ( -7.892574838092353495, -1.309761382309196032, 14.00000000000000000 ) ) ;
#2143 = CARTESIAN_POINT ( 'NONE',  ( 2.406079317367887160, 6.392288322179701332, 1.999999999999998224 ) ) ;
#2144 = PRODUCT_DEFINITION_FORMATION_WITH_SPECIFIED_SOURCE ( 'ANY', '', #5145, .NOT_KNOWN. ) ;
#2145 = DIRECTION ( 'NONE',  ( 0.000000000000000000, 0.000000000000000000, -1.000000000000000000 ) ) ;
#2146 = CARTESIAN_POINT ( 'NONE',  ( 7.925371078819432036, 2.990572132494779378, 14.00000000000000000 ) ) ;
#2147 = ORIENTED_EDGE ( 'NONE', *, *, #4585, .T. ) ;
#2148 = PRODUCT_RELATED_PRODUCT_CATEGORY ( 'part', '', ( #2846 ) ) ;
#2149 = DIRECTION ( 'NONE',  ( -0.000000000000000000, -0.000000000000000000, -1.000000000000000000 ) ) ;
#2150 = CARTESIAN_POINT ( 'NONE',  ( -1.189470317277863565, -7.202885406307538041, 13.99999999999999645 ) ) ;
#2151 = AXIS2_PLACEMENT_3D ( 'NONE', #4670, #2424, #5070 ) ;
#2152 = APPLICATION_PROTOCOL_DEFINITION ( 'draft international standard', 'automotive_design', 1998, #5414 ) ;
#2153 = CARTESIAN_POINT ( 'NONE',  ( -5.048038583874033591, -7.300734008993713609, 1.999999999999998224 ) ) ;
#2154 = CARTESIAN_POINT ( 'NONE',  ( 6.033242055734851839, 5.122103984031729063, 1.999999999999998224 ) ) ;
#2155 = CARTESIAN_POINT ( 'NONE',  ( 6.679452517770527287, -4.623421500472437273, 13.99999999999999645 ) ) ;
#2156 = CIRCLE ( 'NONE', #588, 23.00000000000000000 ) ;
#2157 = CARTESIAN_POINT ( 'NONE',  ( 5.000000000000000000, 5.000000000000022204, 5.000000000000000000 ) ) ;
#2158 = CARTESIAN_POINT ( 'NONE',  ( -8.929154442179981999, -4.413097966322209409, 1.999999999999998224 ) ) ;
#2159 = AXIS2_PLACEMENT_3D ( 'NONE', #2408, #4540, #3197 ) ;
#2160 = CARTESIAN_POINT ( 'NONE',  ( 5.500000000000000000, 0.000000000000000000, 1.999999999999998224 ) ) ;
#2161 = CARTESIAN_POINT ( 'NONE',  ( 0.000000000000000000, 0.000000000000000000, -8.000000000000000000 ) ) ;
#2162 = ORIENTED_EDGE ( 'NONE', *, *, #395, .T. ) ;
#2163 = CARTESIAN_POINT ( 'NONE',  ( 23.24999999999999645, -8.485281374238580199, -4.000000000000000000 ) ) ;
#2164 = AXIS2_PLACEMENT_3D ( 'NONE', #3290, #3378, #4692 ) ;
#2165 = CARTESIAN_POINT ( 'NONE',  ( 8.952336951391263398, 1.032601321559317276, 13.99999999999999645 ) ) ;
#2166 = SURFACE_SIDE_STYLE ('',( #3974 ) ) ;
#2168 = VERTEX_POINT ( 'NONE', #4938 ) ;
#2167 = VECTOR ( 'NONE', #2531, 1000.000000000000000 ) ;
#2169 = CARTESIAN_POINT ( 'NONE',  ( 0.000000000000000000, 0.000000000000000000, -8.000000000000000000 ) ) ;
#2170 = VERTEX_POINT ( 'NONE', #128 ) ;
#2171 = CARTESIAN_POINT ( 'NONE',  ( 21.74999999999999645, -30.00000000000000000, 4.000000000000001776 ) ) ;
#2172 = EDGE_CURVE ( 'NONE', #2002, #3473, #2406, .T. ) ;
#2173 = CARTESIAN_POINT ( 'NONE',  ( -2.415560149437796511, -8.486491385245610530, 14.00000000000000000 ) ) ;
#2174 = CARTESIAN_POINT ( 'NONE',  ( -0.7077576507784110182, 10.75210906117156995, 13.99999999999999645 ) ) ;
#2175 = AXIS2_PLACEMENT_3D ( 'NONE', #920, #1868, #110 ) ;
#2176 = DIRECTION ( 'NONE',  ( 0.000000000000000000, 0.000000000000000000, 1.000000000000000000 ) ) ;
#2177 = CARTESIAN_POINT ( 'NONE',  ( 0.5141566911144540564, -7.748312628312728378, 14.00000000000000000 ) ) ;
#2178 = ORIENTED_EDGE ( 'NONE', *, *, #1405, .T. ) ;
#2179 = CIRCLE ( 'NONE', #2729, 23.00000000000000000 ) ;
#2180 = DIRECTION ( 'NONE',  ( -1.000000000000000000, -0.000000000000000000, -0.000000000000000000 ) ) ;
#2181 = CARTESIAN_POINT ( 'NONE',  ( 6.180183843827204093, 3.174252413088802793, 13.99999999999999645 ) ) ;
#2182 = CIRCLE ( 'NONE', #2915, 25.00000000000000000 ) ;
#2183 = CARTESIAN_POINT ( 'NONE',  ( -8.547479018124427341, -2.754496926847987748, 1.999999999999998224 ) ) ;
#2184 = ORIENTED_EDGE ( 'NONE', *, *, #4565, .F. ) ;
#2185 = CARTESIAN_POINT ( 'NONE',  ( 5.586635445632133212, -4.430858740432559451, 1.999999999999998224 ) ) ;
#2186 = AXIS2_PLACEMENT_3D ( 'NONE', #4834, #484, #1301 ) ;
#2187 = PLANE ( 'NONE',  #1883 ) ;
#2188 = SURFACE_SIDE_STYLE ('',( #5242 ) ) ;
#2189 = DIRECTION ( 'NONE',  ( 0.000000000000000000, 0.000000000000000000, 1.000000000000000000 ) ) ;
#2190 = CARTESIAN_POINT ( 'NONE',  ( -3.922355934210176809, -4.464780306276820099, 1.999999999999998224 ) ) ;
#2191 = CARTESIAN_POINT ( 'NONE',  ( 5.000000000000000000, 5.000000000000022204, 8.000000000000000000 ) ) ;
#2192 = ORIENTED_EDGE ( 'NONE', *, *, #3796, .T. ) ;
#2193 = DIRECTION ( 'NONE',  ( 0.000000000000000000, 0.000000000000000000, -1.000000000000000000 ) ) ;
#2194 = CARTESIAN_POINT ( 'NONE',  ( 1.176163838800443395, -10.19826953922044765, 13.99999999999999645 ) ) ;
#2195 = ADVANCED_FACE ( 'NONE', ( #669 ), #2420, .T. ) ;
#2196 = CARTESIAN_POINT ( 'NONE',  ( 1.300000000000000044, -0.7216878364870319418, 1.249999999999999778 ) ) ;
#2197 = EDGE_CURVE ( 'NONE', #2597, #2807, #5067, .T. ) ;
#2198 = ORIENTED_EDGE ( 'NONE', *, *, #3915, .F. ) ;
#2199 = DIRECTION ( 'NONE',  ( 0.2000000000000004552, 0.9797958971132711969, 0.000000000000000000 ) ) ;
#2200 = ORIENTED_EDGE ( 'NONE', *, *, #2956, .F. ) ;
#2201 = ORIENTED_EDGE ( 'NONE', *, *, #5546, .F. ) ;
#2202 = CARTESIAN_POINT ( 'NONE',  ( -7.652305818843811558, 2.590529227167490234, 14.00000000000000000 ) ) ;
#2203 = CARTESIAN_POINT ( 'NONE',  ( 10.98697916625460991, 0.8999353979983718554, 13.99999999999999645 ) ) ;
#2204 = DIRECTION ( 'NONE',  ( 0.000000000000000000, 0.000000000000000000, -1.000000000000000000 ) ) ;
#2205 = CARTESIAN_POINT ( 'NONE',  ( 2.543939756934300966, 7.929199913827024382, 14.00000000000000000 ) ) ;
#2206 = ORIENTED_EDGE ( 'NONE', *, *, #3504, .F. ) ;
#2207 = CARTESIAN_POINT ( 'NONE',  ( 2.810994617404584783, -9.846529629019117991, 1.999999999999998224 ) ) ;
#2208 = CARTESIAN_POINT ( 'NONE',  ( 1.300000000000000044, 0.000000000000000000, -1.250000000000000000 ) ) ;
#2209 = EDGE_CURVE ( 'NONE', #5308, #2034, #2251, .T. ) ;
#2210 = CARTESIAN_POINT ( 'NONE',  ( 7.025143070632195119, -0.1151745751371588272, 13.99999999999999645 ) ) ;
#2211 = APPLICATION_PROTOCOL_DEFINITION ( 'draft international standard', 'automotive_design', 1998, #2102 ) ;
#2212 = CARTESIAN_POINT ( 'NONE',  ( -4.983290658055095967, 7.721050520723657051, 1.999999999999998224 ) ) ;
#2213 = CARTESIAN_POINT ( 'NONE',  ( -7.364573508975982286, 1.714675912027187943, 1.999999999999998224 ) ) ;
#2214 = CARTESIAN_POINT ( 'NONE',  ( 17.99999999999999289, -15.01665741768121443, 8.000000000000000000 ) ) ;
#2215 = FILL_AREA_STYLE_COLOUR ( '', #3606 ) ;
#2216 = SPHERICAL_SURFACE ( 'NONE', #681, 4.324969328314201888 ) ;
#2217 = CARTESIAN_POINT ( 'NONE',  ( 4.443413384189978110, 4.597174039215664365, 1.999999999999998224 ) ) ;
#2218 = FACE_OUTER_BOUND ( 'NONE', #2738, .T. ) ;
#2219 = EDGE_LOOP ( 'NONE', ( #4311, #3579, #2918, #5649 ) ) ;
#2220 = ADVANCED_FACE ( 'NONE', ( #2505 ), #2940, .T. ) ;
#2221 = CARTESIAN_POINT ( 'NONE',  ( -10.53467355220997526, 0.3418899515811328338, 13.99999999999999645 ) ) ;
#2222 = DIRECTION ( 'NONE',  ( -0.000000000000000000, -0.000000000000000000, 1.000000000000000000 ) ) ;
#2223 = ORIENTED_EDGE ( 'NONE', *, *, #2442, .F. ) ;
#2224 = VERTEX_POINT ( 'NONE', #1189 ) ;
#2225 = CARTESIAN_POINT ( 'NONE',  ( 7.017208779832877497, -5.019401656905778886, 14.00000000000000000 ) ) ;
#2226 = CARTESIAN_POINT ( 'NONE',  ( 4.585040342817966241, 6.402697129001492904, 1.999999999999998224 ) ) ;
#2227 = LINE ( 'NONE', #4362, #960 ) ;
#2228 = EDGE_CURVE ( 'NONE', #247, #4608, #873, .T. ) ;
#2229 = CARTESIAN_POINT ( 'NONE',  ( -0.2798806129217078498, -8.779921314117062892, 14.00000000000000000 ) ) ;
#2230 = EDGE_LOOP ( 'NONE', ( #667, #1223, #4104, #567 ) ) ;
#2231 = CARTESIAN_POINT ( 'NONE',  ( 5.279590631141700463, 9.498297537454860162, 1.999999999999998224 ) ) ;
#2232 = DIRECTION ( 'NONE',  ( -0.000000000000000000, -0.000000000000000000, 1.000000000000000000 ) ) ;
#2233 = CARTESIAN_POINT ( 'NONE',  ( 4.914575889516433094, -3.754581871930561032, 13.99999999999999645 ) ) ;
#2234 = CARTESIAN_POINT ( 'NONE',  ( -3.672794075660469559, 8.451992513476518809, 1.999999999999998224 ) ) ;
#2235 = ADVANCED_FACE ( 'NONE', ( #4152 ), #1126, .T. ) ;
#2236 = CARTESIAN_POINT ( 'NONE',  ( -2.721086536275891810, 7.222755814214461445, 1.999999999999998224 ) ) ;
#2237 = DIRECTION ( 'NONE',  ( -0.000000000000000000, 1.000000000000000000, 0.000000000000000000 ) ) ;
#2238 = UNCERTAINTY_MEASURE_WITH_UNIT (LENGTH_MEASURE( 1.000000000000000082E-05 ), #397, 'distance_accuracy_value', 'NONE');
#2239 = PRESENTATION_LAYER_ASSIGNMENT (  '', '', ( #3986 ) ) ;
#2240 = DIRECTION ( 'NONE',  ( -0.000000000000000000, -0.000000000000000000, 1.000000000000000000 ) ) ;
#2241 = CARTESIAN_POINT ( 'NONE',  ( 1.492118473828444536, -5.588909376072070501, 1.999999999999998224 ) ) ;
#2242 = LINE ( 'NONE', #862, #5205 ) ;
#2243 = DIRECTION ( 'NONE',  ( -4.364351673553916694E-15, 1.000000000000000000, 0.000000000000000000 ) ) ;
#2244 = ORIENTED_EDGE ( 'NONE', *, *, #1245, .T. ) ;
#2245 = PLANE ( 'NONE',  #607 ) ;
#2246 = AXIS2_PLACEMENT_3D ( 'NONE', #3764, #4228, #4682 ) ;
#2247 = DIRECTION ( 'NONE',  ( -0.000000000000000000, -0.000000000000000000, 1.000000000000000000 ) ) ;
#2248 = PLANE ( 'NONE',  #2058 ) ;
#2249 = CARTESIAN_POINT ( 'NONE',  ( 0.000000000000000000, 0.000000000000000000, -58.22539674441618018 ) ) ;
#2250 = EDGE_LOOP ( 'NONE', ( #2639, #4690, #2162 ) ) ;
#2251 = CIRCLE ( 'NONE', #318, 15.00000000000000000 ) ;
#2252 = ORIENTED_EDGE ( 'NONE', *, *, #1780, .F. ) ;
#2253 = CARTESIAN_POINT ( 'NONE',  ( 8.256732931686221022, 4.597988481711512421, 14.00000000000000000 ) ) ;
#2254 = CARTESIAN_POINT ( 'NONE',  ( 7.565999024956892249, -2.848076369834589450, 1.999999999999998224 ) ) ;
#2255 = AXIS2_PLACEMENT_3D ( 'NONE', #617, #5537, #3692 ) ;
#2256 = CARTESIAN_POINT ( 'NONE',  ( -8.013356705133178437, 0.6503825268544296545, 1.999999999999998224 ) ) ;
#2257 = CARTESIAN_POINT ( 'NONE',  ( -1.480145937554535385, 8.115026467927430431, 14.00000000000000000 ) ) ;
#2258 = VERTEX_POINT ( 'NONE', #2831 ) ;
#2259 = CARTESIAN_POINT ( 'NONE',  ( -9.742306995815773973, -3.848972158781406083, 1.999999999999998224 ) ) ;
#2260 = CARTESIAN_POINT ( 'NONE',  ( 5.460516619045268527, 3.400499599735717915, 14.00000000000000000 ) ) ;
#2261 = CARTESIAN_POINT ( 'NONE',  ( -7.245889760505164645, 4.668767092638694827, 13.99999999999999645 ) ) ;
#2262 = VECTOR ( 'NONE', #313, 1000.000000000000000 ) ;
#2263 = CARTESIAN_POINT ( 'NONE',  ( 4.585040342817689130, 6.402697129001494680, 13.99999999999999645 ) ) ;
#2264 = CARTESIAN_POINT ( 'NONE',  ( 7.017208779832875720, -5.019401656906101294, 1.999999999999998224 ) ) ;
#2265 = ADVANCED_FACE ( 'NONE', ( #2481 ), #3319, .F. ) ;
#2266 = CIRCLE ( 'NONE', #2355, 25.00000000000000355 ) ;
#2267 = CARTESIAN_POINT ( 'NONE',  ( -7.519441789400336695, 0.4931591957933217363, 1.999999999999998224 ) ) ;
#2268 = CARTESIAN_POINT ( 'NONE',  ( 13.00000000000000178, 0.000000000000000000, 12.00000000000000000 ) ) ;
#2269 = LINE ( 'NONE', #4453, #2615 ) ;
#2270 = CARTESIAN_POINT ( 'NONE',  ( -5.183646570197097958, -3.010418922387011698, 1.999999999999998224 ) ) ;
#2271 = AXIS2_PLACEMENT_3D ( 'NONE', #5270, #3087, #2741 ) ;
#2272 = DIRECTION ( 'NONE',  ( -1.000000000000000000, 0.000000000000000000, 0.000000000000000000 ) ) ;
#2273 = DIRECTION ( 'NONE',  ( -0.000000000000000000, -0.000000000000000000, 1.000000000000000000 ) ) ;
#2274 = DIRECTION ( 'NONE',  ( -0.01205169166640770832, -0.9999273757268464236, -2.258590485605784177E-18 ) ) ;
#2275 = CARTESIAN_POINT ( 'NONE',  ( 7.631804465920718705, -6.689046765414282447, 13.99999999999999645 ) ) ;
#2276 = FACE_OUTER_BOUND ( 'NONE', #2747, .T. ) ;
#2277 = CARTESIAN_POINT ( 'NONE',  ( 18.00000000000000000, 1.553654299240552096E-15, -16.41957833606399930 ) ) ;
#2278 = EDGE_LOOP ( 'NONE', ( #2198, #3250, #5233, #4878 ) ) ;
#2279 = ORIENTED_EDGE ( 'NONE', *, *, #4046, .F. ) ;
#2280 = CARTESIAN_POINT ( 'NONE',  ( 8.549805251451807919, -4.382211019330642721, 14.00000000000000000 ) ) ;
#2281 = CARTESIAN_POINT ( 'NONE',  ( 4.793600759081159346, 4.956424179878264447, 1.999999999999998224 ) ) ;
#2282 = CARTESIAN_POINT ( 'NONE',  ( -6.185289998984973003, -6.402116997106289453, 1.999999999999998224 ) ) ;
#2283 = CARTESIAN_POINT ( 'NONE',  ( -6.700137237868793783, -5.881230172876196427, 14.00000000000000000 ) ) ;
#2284 = ORIENTED_EDGE ( 'NONE', *, *, #5599, .F. ) ;
#2285 = CARTESIAN_POINT ( 'NONE',  ( 3.158576809044846279, 9.313732666428188978, 1.999999999999998224 ) ) ;
#2286 = CARTESIAN_POINT ( 'NONE',  ( 1.300000000000000044, -0.7216878364870319418, 1.249999999999999778 ) ) ;
#2287 = CARTESIAN_POINT ( 'NONE',  ( 2.701324588234351953, 8.405562337868641265, 13.99999999999999645 ) ) ;
#2288 = ADVANCED_FACE ( 'NONE', ( #263 ), #4266, .T. ) ;
#2289 = CARTESIAN_POINT ( 'NONE',  ( -7.091148812992124739, -4.571561645351811976, 13.99999999999999645 ) ) ;
#2290 = CARTESIAN_POINT ( 'NONE',  ( -6.048456868091351524, 0.8014113234714785872, 14.00000000000000000 ) ) ;
#2291 = CARTESIAN_POINT ( 'NONE',  ( 1.870926337630253622, -8.025887876971653512, 1.999999999999998224 ) ) ;
#2292 = EDGE_CURVE ( 'NONE', #4697, #4516, #1515, .T. ) ;
#2293 = FACE_OUTER_BOUND ( 'NONE', #3783, .T. ) ;
#2294 =( NAMED_UNIT ( * ) SI_UNIT ( $, .STERADIAN. ) SOLID_ANGLE_UNIT ( ) );
#2295 = CARTESIAN_POINT ( 'NONE',  ( 6.315449825284093599, 1.474116854620456163, 1.999999999999998224 ) ) ;
#2296 = EDGE_LOOP ( 'NONE', ( #1672, #544, #2339, #5529 ) ) ;
#2297 = CARTESIAN_POINT ( 'NONE',  ( -0.3669926094919909731, -5.824518274481597757, 1.999999999999998224 ) ) ;
#2298 = DIRECTION ( 'NONE',  ( -0.000000000000000000, -0.000000000000000000, 1.000000000000000000 ) ) ;
#2299 = DIRECTION ( 'NONE',  ( 0.000000000000000000, 0.000000000000000000, -1.000000000000000000 ) ) ;
#2300 = EDGE_CURVE ( 'NONE', #1028, #2224, #1429, .T. ) ;
#2301 = UNCERTAINTY_MEASURE_WITH_UNIT (LENGTH_MEASURE( 1.000000000000000082E-05 ), #4064, 'distance_accuracy_value', 'NONE');
#2302 = CARTESIAN_POINT ( 'NONE',  ( 8.671201137382265500, 6.657490096169393468, 13.99999999999999645 ) ) ;
#2303 = DIRECTION ( 'NONE',  ( 1.000000000000000000, 0.000000000000000000, 0.000000000000000000 ) ) ;
#2304 = LINE ( 'NONE', #5390, #54 ) ;
#2305 = ORIENTED_EDGE ( 'NONE', *, *, #1524, .F. ) ;
#2306 = EDGE_CURVE ( 'NONE', #928, #5593, #138, .T. ) ;
#2307 = ORIENTED_EDGE ( 'NONE', *, *, #5183, .F. ) ;
#2308 = CARTESIAN_POINT ( 'NONE',  ( 5.519166806814065573, -7.959527472086049826, 14.00000000000000000 ) ) ;
#2309 = CARTESIAN_POINT ( 'NONE',  ( 4.366464973618271905, -5.686602709308029802, 1.999999999999998224 ) ) ;
#2310 = CARTESIAN_POINT ( 'NONE',  ( -5.581220830680290845, 5.949058968288200688, 1.999999999999998224 ) ) ;
#2311 = CARTESIAN_POINT ( 'NONE',  ( -4.354965481614498479, -8.841480220785717492, 14.00000000000000000 ) ) ;
#2312 = ORIENTED_EDGE ( 'NONE', *, *, #4232, .F. ) ;
#2313 = CARTESIAN_POINT ( 'NONE',  ( 3.917689075872947235, 9.035181080458078995, 1.999999999999998224 ) ) ;
#2314 = LINE ( 'NONE', #3695, #808 ) ;
#2315 = CARTESIAN_POINT ( 'NONE',  ( -4.060726170632903198, -7.305992298388080286, 13.99999999999999645 ) ) ;
#2316 = MECHANICAL_DESIGN_GEOMETRIC_PRESENTATION_REPRESENTATION (  '', ( #5073 ), #2962 ) ;
#2317 = CARTESIAN_POINT ( 'NONE',  ( 4.264126983937991611, 9.433107915010285893, 1.999999999999998224 ) ) ;
#2318 = EDGE_LOOP ( 'NONE', ( #4210, #3063 ) ) ;
#2319 = PRODUCT_DEFINITION_FORMATION_WITH_SPECIFIED_SOURCE ( 'ANY', '', #5046, .NOT_KNOWN. ) ;
#2320 = CARTESIAN_POINT ( 'NONE',  ( 7.422282976138727228, -5.315384720684046549, 1.999999999999998224 ) ) ;
#2321 = CARTESIAN_POINT ( 'NONE',  ( 10.20000000000000107, 0.000000000000000000, 0.000000000000000000 ) ) ;
#2322 = CARTESIAN_POINT ( 'NONE',  ( -3.715337444063474770, -5.771435016728991840, 1.999999999999998224 ) ) ;
#2323 = ORIENTED_EDGE ( 'NONE', *, *, #500, .F. ) ;
#2324 = CARTESIAN_POINT ( 'NONE',  ( 5.648567055624510225, 4.800053419556092216, 1.999999999999998224 ) ) ;
#2325 = FACE_OUTER_BOUND ( 'NONE', #2250, .T. ) ;
#2326 = CARTESIAN_POINT ( 'NONE',  ( -6.551010013419181988, 0.8677952034721571062, 13.99999999999999645 ) ) ;
#2327 = MECHANICAL_DESIGN_GEOMETRIC_PRESENTATION_REPRESENTATION (  '', ( #5638 ), #3526 ) ;
#2328 = CARTESIAN_POINT ( 'NONE',  ( 0.000000000000000000, 0.000000000000000000, -3.300000000000000266 ) ) ;
#2329 = AXIS2_PLACEMENT_3D ( 'NONE', #360, #1797, #2664 ) ;
#2330 = DIRECTION ( 'NONE',  ( 0.000000000000000000, 0.000000000000000000, 1.000000000000000000 ) ) ;
#2331 = ORIENTED_EDGE ( 'NONE', *, *, #1295, .F. ) ;
#2332 = CARTESIAN_POINT ( 'NONE',  ( 1.300000000000000044, 0.7216878364870328300, -1.250000000000000000 ) ) ;
#2333 = CARTESIAN_POINT ( 'NONE',  ( -1.515482495401828000, 9.129776367295956874, 14.00000000000000000 ) ) ;
#2334 = CARTESIAN_POINT ( 'NONE',  ( 5.887534416617370425, 3.663839002572738313, 1.999999999999998224 ) ) ;
#2335 = AXIS2_PLACEMENT_3D ( 'NONE', #1055, #2348, #542 ) ;
#2336 = CARTESIAN_POINT ( 'NONE',  ( -7.966005157978614193, 4.422220743486963812, 1.999999999999998224 ) ) ;
#2337 = CARTESIAN_POINT ( 'NONE',  ( -7.963215149404076598, -4.094909132697305054, 14.00000000000000000 ) ) ;
#2338 =( GEOMETRIC_REPRESENTATION_CONTEXT ( 3 ) GLOBAL_UNCERTAINTY_ASSIGNED_CONTEXT ( ( #3315 ) ) GLOBAL_UNIT_ASSIGNED_CONTEXT ( ( #5388, #4520, #3660 ) ) REPRESENTATION_CONTEXT ( 'NONE', 'WORKASPACE' ) );
#2339 = ORIENTED_EDGE ( 'NONE', *, *, #4283, .T. ) ;
#2340 = CARTESIAN_POINT ( 'NONE',  ( 17.99999999999999289, -17.34935157289748631, 8.000000000000000000 ) ) ;
#2341 = CARTESIAN_POINT ( 'NONE',  ( 0.2014543481397604030, 6.272771216426900942, 14.00000000000000000 ) ) ;
#2342 = CARTESIAN_POINT ( 'NONE',  ( -7.884571930971329579, 3.418633173532294123, 13.99999999999999645 ) ) ;
#2343 = VECTOR ( 'NONE', #2199, 999.9999999999998863 ) ;
#2344 = CARTESIAN_POINT ( 'NONE',  ( -9.986481889893736863, 1.144076113142370899, 1.999999999999998224 ) ) ;
#2345 = EDGE_LOOP ( 'NONE', ( #1480, #3288, #1331, #227, #3686 ) ) ;
#2346 = AXIS2_PLACEMENT_3D ( 'NONE', #1990, #3744, #5097 ) ;
#2347 = CARTESIAN_POINT ( 'NONE',  ( 4.074896204546095468, -8.256886768008961042, 1.999999999999998224 ) ) ;
#2348 = DIRECTION ( 'NONE',  ( 0.000000000000000000, 0.000000000000000000, -1.000000000000000000 ) ) ;
#2349 = VECTOR ( 'NONE', #4098, 1000.000000000000000 ) ;
#2350 = CARTESIAN_POINT ( 'NONE',  ( -5.370374743918785221, 4.702532619530842339, 1.999999999999998224 ) ) ;
#2351 = EDGE_LOOP ( 'NONE', ( #2443, #4417, #950, #4511 ) ) ;
#2352 = CARTESIAN_POINT ( 'NONE',  ( -6.317162512443194267, 3.238855812894541941, 1.999999999999998224 ) ) ;
#2353 = CARTESIAN_POINT ( 'NONE',  ( 5.400000000000002132, 26.45448922205832432, 4.000000000000000000 ) ) ;
#2354 = EDGE_CURVE ( 'NONE', #4137, #5065, #5382, .T. ) ;
#2355 = AXIS2_PLACEMENT_3D ( 'NONE', #2564, #4265, #3427 ) ;
#2356 =( LENGTH_UNIT ( ) NAMED_UNIT ( * ) SI_UNIT ( .MILLI., .METRE. ) );
#2357 = VECTOR ( 'NONE', #1167, 1000.000000000000000 ) ;
#2358 = EDGE_CURVE ( 'NONE', #2168, #4001, #1960, .T. ) ;
#2359 = APPLICATION_CONTEXT ( 'automotive_design' ) ;
#2360 = SURFACE_STYLE_FILL_AREA ( #4094 ) ;
#2361 = CARTESIAN_POINT ( 'NONE',  ( 0.000000000000000000, 0.000000000000000000, 5.000000000000000000 ) ) ;
#2362 = ORIENTED_EDGE ( 'NONE', *, *, #3391, .T. ) ;
#2363 = DIRECTION ( 'NONE',  ( 1.000000000000000000, 0.000000000000000000, 0.000000000000000000 ) ) ;
#2364 = CARTESIAN_POINT ( 'NONE',  ( 2.992331685656917539, 8.840389773664524498, 14.00000000000000000 ) ) ;
#2365 = CARTESIAN_POINT ( 'NONE',  ( 2.701324588234195190, 8.405562337868014211, 1.999999999999998224 ) ) ;
#2366 = AXIS2_PLACEMENT_3D ( 'NONE', #519, #2677, #921 ) ;
#2367 = EDGE_CURVE ( 'NONE', #3324, #3442, #4885, .T. ) ;
#2368 = B_SPLINE_CURVE_WITH_KNOTS ( 'NONE', 3,
 ( #5269, #3142, #3571, #2703, #2623, #3086, #1840, #2297, #4377, #3116, #2190, #3943, #1324, #2740, #979, #1, #483, #4457, #518, #1753, #4833, #4030, #5351, #1409, #4919, #892, #4402, #3538, #458, #2217, #2676, #3968, #1358, #4863, #4428, #690, #1089, #1984, #4602, #4120, #3310, #1006, #568, #5060, #3704, #3680, #5435, #3737, #2875, #2384, #2444, #603, #1029, #3202, #4087, #4999, #255, #4204, #2014, #1469, #1118, #1490, #2787, #2765, #4517, #2352, #198, #4628, #172, #3281, #140, #5465, #4573, #1060, #4971, #5522, #633, #1924, #2850, #4949, #3768, #2324, #1898, #3657, #4543, #5410, #3225, #4143, #1951, #1522, #3251, #5034, #661, #2821, #2412, #4173, #228, #5496, #1557, #2905, #4658, #1580, #3339, #5091, #1147, #2802, #4441, #4013, #3211, #3127, #70, #2369, #615, #2256, #3639, #3667, #3182, #1455, #497, #2310, #4554, #4042, #1853, #1826, #183, #4981, #2719, #1936, #5395, #991, #156, #4932, #1912, #1372, #4876, #583, #1881, #3584, #2686, #4129, #5337, #5421, #3155, #1477, #3609, #97, #932, #1395, #4901, #4102, #5365, #961, #4471, #1422, #3690, #2774, #531, #2282, #4959, #3234, #4528, #2750, #4502, #1041, #555, #4070, #122, #1016, #2336, #5214, #3029, #1644, #1695, #1073, #3264, #1212, #2998, #1501, #4712, #776, #2835, #4774, #2073, #1269, #3400, #5043, #4587, #3295, #807, #5446, #2499, #1538, #5583, #835, #5153, #1184, #2964, #2528, #3830, #5175, #2128, #2587, #3451, #645, #210, #2935, #311, #1236, #4346, #4291, #399, #2158, #4687, #344, #2099, #4260, #5015, #3857, #5608, #2397, #369, #747, #3718, #4156, #1669, #5478, #3424, #4743, #2560, #1963, #3884, #4320, #5636, #1323, #3084, #4487, #3996, #4029, #1384, #5324, #1779, #4455 ),
 .UNSPECIFIED., .F., .F.,
 ( 4, 2, 2, 2, 2, 2, 2, 2, 2, 2, 2, 2, 2, 2, 2, 2, 2, 2, 2, 2, 2, 2, 2, 2, 2, 2, 2, 2, 2, 2, 2, 2, 2, 2, 2, 2, 2, 2, 2, 2, 2, 2, 2, 2, 2, 2, 2, 2, 2, 2, 2, 2, 2, 2, 2, 2, 2, 2, 2, 2, 2, 2, 2, 2, 2, 2, 2, 2, 2, 2, 2, 2, 2, 2, 2, 2, 2, 2, 2, 2, 2, 2, 2, 2, 2, 2, 2, 2, 2, 2, 2, 2, 2, 2, 2, 2, 2, 2, 2, 2, 2, 2, 2, 2, 2, 2, 2, 2, 2, 2, 2, 2, 2, 2, 2, 2, 2, 2, 2, 2, 4 ),
 ( 0.000000000000000000, 0.01562500000000000000, 0.03125000000000000000, 0.04687500000000000000, 0.06250000000000000000, 0.07812500000000000000, 0.09375000000000000000, 0.1093750000000000000, 0.1250000000000000000, 0.1328125000000000000, 0.1406250000000000000, 0.1484375000000000000, 0.1562500000000000000, 0.1640625000000000000, 0.1718750000000000000, 0.1796875000000000000, 0.1875000000000000000, 0.1953125000000000000, 0.2031250000000000000, 0.2109375000000000000, 0.2187500000000000000, 0.2265625000000000000, 0.2343750000000000000, 0.2421875000000000000, 0.2500000000000000000, 0.2578125000000000000, 0.2656250000000000000, 0.2734375000000000000, 0.2812500000000000000, 0.2890625000000000000, 0.2968750000000000000, 0.3046875000000000000, 0.3125000000000000000, 0.3203125000000000000, 0.3281250000000000000, 0.3359375000000000000, 0.3437500000000000000, 0.3515625000000000000, 0.3593750000000000000, 0.3671875000000000000, 0.3750000000000000000, 0.3828125000000000000, 0.3906250000000000000, 0.3984375000000000000, 0.4062500000000000000, 0.4140625000000000000, 0.4218750000000000000, 0.4296875000000000000, 0.4375000000000000000, 0.4453125000000000000, 0.4531250000000000000, 0.4609375000000000000, 0.4687500000000000000, 0.4765625000000000000, 0.4843750000000000000, 0.4921875000000000000, 0.5000000000000000000, 0.5078125000000000000, 0.5156250000000000000, 0.5234375000000000000, 0.5312500000000000000, 0.5390625000000000000, 0.5468750000000000000, 0.5546875000000000000, 0.5625000000000000000, 0.5703125000000000000, 0.5781250000000000000, 0.5859375000000000000, 0.5937500000000000000, 0.6015625000000000000, 0.6093750000000000000, 0.6171875000000000000, 0.6250000000000000000, 0.6328125000000000000, 0.6406250000000000000, 0.6484375000000000000, 0.6562500000000000000, 0.6640625000000000000, 0.6718750000000000000, 0.6796875000000000000, 0.6875000000000000000, 0.6953125000000000000, 0.7031250000000000000, 0.7109375000000000000, 0.7187500000000000000, 0.7265625000000000000, 0.7343750000000000000, 0.7421875000000000000, 0.7500000000000000000, 0.7578125000000000000, 0.7656250000000000000, 0.7734375000000000000, 0.7812500000000000000, 0.7890625000000000000, 0.7968750000000000000, 0.8046875000000000000, 0.8125000000000000000, 0.8203125000000000000, 0.8281250000000000000, 0.8359375000000000000, 0.8437500000000000000, 0.8515625000000000000, 0.8593750000000000000, 0.8671875000000000000, 0.8750000000000000000, 0.8828125000000000000, 0.8906250000000000000, 0.8984375000000000000, 0.9062500000000000000, 0.9140625000000000000, 0.9218750000000000000, 0.9296875000000000000, 0.9375000000000000000, 0.9453125000000000000, 0.9531250000000000000, 0.9609375000000000000, 0.9687500000000000000, 0.9765625000000000000, 0.9843750000000000000, 0.9921875000000000000, 1.000000000000000000 ),
 .UNSPECIFIED. ) ;
#2369 = CARTESIAN_POINT ( 'NONE',  ( -7.892574838092051515, -1.309761382309195366, 1.999999999999998224 ) ) ;
#2370 = CARTESIAN_POINT ( 'NONE',  ( -8.763921109941536614, 2.343993041296470903, 14.00000000000000000 ) ) ;
#2371 = CARTESIAN_POINT ( 'NONE',  ( 5.000000000000000000, 5.000000000000022204, -5.000000000000000000 ) ) ;
#2372 = ORIENTED_EDGE ( 'NONE', *, *, #2842, .T. ) ;
#2373 = CARTESIAN_POINT ( 'NONE',  ( 9.199536834907135585, 5.930433524309127513, 1.999999999999998224 ) ) ;
#2374 = CARTESIAN_POINT ( 'NONE',  ( -3.595699629853522872, 5.016010494498949868, 14.00000000000000000 ) ) ;
#2375 = CARTESIAN_POINT ( 'NONE',  ( -1.342170334697156742, -10.21728332006373030, 13.99999999999999645 ) ) ;
#2376 = CARTESIAN_POINT ( 'NONE',  ( 9.602236826901936695, 4.172718697305983326, 1.999999999999998224 ) ) ;
#2377 = VERTEX_POINT ( 'NONE', #2732 ) ;
#2378 = CARTESIAN_POINT ( 'NONE',  ( 4.326322805049506393, -6.952463250691141461, 1.999999999999998224 ) ) ;
#2379 = EDGE_CURVE ( 'NONE', #4336, #3693, #1382, .T. ) ;
#2380 = CARTESIAN_POINT ( 'NONE',  ( 9.809999999999998721, 0.000000000000000000, 1.999999999999999556 ) ) ;
#2381 = PRESENTATION_STYLE_ASSIGNMENT (( #599 ) ) ;
#2382 = CARTESIAN_POINT ( 'NONE',  ( 4.848934754808810865, -4.539135254905419359, 1.999999999999998224 ) ) ;
#2383 = ORIENTED_EDGE ( 'NONE', *, *, #4995, .F. ) ;
#2384 = CARTESIAN_POINT ( 'NONE',  ( -0.5497243705170606898, -6.763214047005217999, 1.999999999999998224 ) ) ;
#2385 = DIRECTION ( 'NONE',  ( 0.000000000000000000, -0.5000000000000001110, -0.8660254037844385966 ) ) ;
#2386 = DIRECTION ( 'NONE',  ( -1.156482317317871478E-16, -1.000000000000000000, 0.000000000000000000 ) ) ;
#2387 = DIRECTION ( 'NONE',  ( -1.000000000000000000, 0.000000000000000000, -0.000000000000000000 ) ) ;
#2388 = DIRECTION ( 'NONE',  ( -0.000000000000000000, -0.000000000000000000, -1.000000000000000000 ) ) ;
#2389 = EDGE_CURVE ( 'NONE', #3723, #1462, #1674, .T. ) ;
#2390 = DIRECTION ( 'NONE',  ( 0.000000000000000000, 1.000000000000000000, 1.224646799147353207E-16 ) ) ;
#2391 = EDGE_LOOP ( 'NONE', ( #1097, #3200, #3123, #2758 ) ) ;
#2392 = PLANE ( 'NONE',  #5300 ) ;
#2393 = DIRECTION ( 'NONE',  ( -0.000000000000000000, -0.000000000000000000, 1.000000000000000000 ) ) ;
#2394 = CARTESIAN_POINT ( 'NONE',  ( 7.422282976138727228, -5.315384720684046549, 1.999999999999998224 ) ) ;
#2395 = CARTESIAN_POINT ( 'NONE',  ( 1.015216742983949372, 7.730330528320555672, 13.99999999999999645 ) ) ;
#2396 =( REPRESENTATION_RELATIONSHIP ('NONE','NONE', #4854, #3487 ) REPRESENTATION_RELATIONSHIP_WITH_TRANSFORMATION ( #3108 )SHAPE_REPRESENTATION_RELATIONSHIP( ) );
#2397 = CARTESIAN_POINT ( 'NONE',  ( -8.765969750979122566, 5.050798838973363125, 1.999999999999998224 ) ) ;
#2398 = CARTESIAN_POINT ( 'NONE',  ( 0.000000000000000000, 0.000000000000000000, 5.000000000000000000 ) ) ;
#2399 = CYLINDRICAL_SURFACE ( 'NONE', #4461, 15.00000000000000000 ) ;
#2400 = ORIENTED_EDGE ( 'NONE', *, *, #1842, .T. ) ;
#2401 = DIRECTION ( 'NONE',  ( -1.000000000000000000, -0.000000000000000000, -0.000000000000000000 ) ) ;
#2402 = CARTESIAN_POINT ( 'NONE',  ( 4.848934754808812642, -4.539135254905673378, 14.00000000000000000 ) ) ;
#2403 = CARTESIAN_POINT ( 'NONE',  ( -9.247353065532886163, -2.155497948345618919, 13.99999999999999645 ) ) ;
#2404 = CARTESIAN_POINT ( 'NONE',  ( 0.1634456542307745064, 10.28566380800474533, 1.999999999999998224 ) ) ;
#2405 = EDGE_LOOP ( 'NONE', ( #2279, #4961 ) ) ;
#2406 = B_SPLINE_CURVE_WITH_KNOTS ( 'NONE', 3,
 ( #560, #4476, #188, #4533, #536, #1047, #1886, #5341, #966, #4559, #2778, #3643, #5400, #1459, #2840, #589, #621, #5426, #2374, #4963, #503, #1020, #3160, #2341, #4987, #4106, #4134, #3671, #1482, #2809, #1941, #2260, #4018, #75, #2724, #713, #3388, #4593, #650, #243, #4162, #1657, #2402, #5513, #736, #1629, #4276, #2087, #2464, #762, #216, #1971, #273, #2512, #3301, #296, #3412, #1199, #327, #3846, #2923, #5569, #5484, #5050, #2431, #5140, #3725, #1572, #677, #4646, #5597, #4221, #4192, #2030, #3785, #2893, #4245, #2948, #5541, #2005, #1546, #1108, #3757, #5076, #2054, #5164, #1596, #1225, #2865, #3328, #3357, #1168, #1134, #4618, #5112, #4675, #2490, #4701, #3813, #1681, #791, #1309, #1253, #3520, #845, #4306, #3436, #1337, #5254, #3013, #381, #2142, #3549, #3067, #3097, #2202, #4845, #2573, #467, #2601, #5228, #3896, #1763, #5653, #903, #4811, #1712, #3954, #4359, #2978, #4727, #415, #5280, #4786, #2660, #2543, #358, #13, #3494, #5621, #2112, #4758, #4412, #2225, #820, #3978, #1285, #3467, #3869, #5193, #4332, #38, #3040, #2173, #3928, #5682, #5309, #4389, #1740, #875, #2634, #444, #1793, #3125, #580, #1878, #4009, #2684, #4551, #66, #3635, #553, #5393, #1933, #5335, #2333, #611, #181, #5362, #2364, #494, #1824, #3607, #3688, #2772, #2253, #1370, #1451, #1475, #4526, #2748, #3209, #1014, #2280, #1418, #3152, #3665, #2308, #3582, #4929, #4127, #3232, #4439, #4873, #4499, #4978, #1393, #4099, #930, #5419, #1038, #2800, #4957, #152, #4899, #958, #2716, #4468, #4068, #527, #4040, #3179, #95, #988, #1850, #119, #1908, #3748, #5100, #2046, #5505, #5040, #3261, #5012, #4610, #2453, #1619, #2857, #5531, #642, #2022, #1099 ),
 .UNSPECIFIED., .F., .F.,
 ( 4, 2, 2, 2, 2, 2, 2, 2, 2, 2, 2, 2, 2, 2, 2, 2, 2, 2, 2, 2, 2, 2, 2, 2, 2, 2, 2, 2, 2, 2, 2, 2, 2, 2, 2, 2, 2, 2, 2, 2, 2, 2, 2, 2, 2, 2, 2, 2, 2, 2, 2, 2, 2, 2, 2, 2, 2, 2, 2, 2, 2, 2, 2, 2, 2, 2, 2, 2, 2, 2, 2, 2, 2, 2, 2, 2, 2, 2, 2, 2, 2, 2, 2, 2, 2, 2, 2, 2, 2, 2, 2, 2, 2, 2, 2, 2, 2, 2, 2, 2, 2, 2, 2, 2, 2, 2, 2, 2, 2, 2, 2, 2, 2, 2, 2, 2, 2, 2, 2, 2, 4 ),
 ( 0.000000000000000000, 0.01562500000000000000, 0.03125000000000000000, 0.04687500000000000000, 0.06250000000000000000, 0.07812500000000000000, 0.09375000000000000000, 0.1093750000000000000, 0.1250000000000000000, 0.1328125000000000000, 0.1406250000000000000, 0.1484375000000000000, 0.1562500000000000000, 0.1640625000000000000, 0.1718750000000000000, 0.1796875000000000000, 0.1875000000000000000, 0.1953125000000000000, 0.2031250000000000000, 0.2109375000000000000, 0.2187500000000000000, 0.2265625000000000000, 0.2343750000000000000, 0.2421875000000000000, 0.2500000000000000000, 0.2578125000000000000, 0.2656250000000000000, 0.2734375000000000000, 0.2812500000000000000, 0.2890625000000000000, 0.2968750000000000000, 0.3046875000000000000, 0.3125000000000000000, 0.3203125000000000000, 0.3281250000000000000, 0.3359375000000000000, 0.3437500000000000000, 0.3515625000000000000, 0.3593750000000000000, 0.3671875000000000000, 0.3750000000000000000, 0.3828125000000000000, 0.3906250000000000000, 0.3984375000000000000, 0.4062500000000000000, 0.4140625000000000000, 0.4218750000000000000, 0.4296875000000000000, 0.4375000000000000000, 0.4453125000000000000, 0.4531250000000000000, 0.4609375000000000000, 0.4687500000000000000, 0.4765625000000000000, 0.4843750000000000000, 0.4921875000000000000, 0.5000000000000000000, 0.5078125000000000000, 0.5156250000000000000, 0.5234375000000000000, 0.5312500000000000000, 0.5390625000000000000, 0.5468750000000000000, 0.5546875000000000000, 0.5625000000000000000, 0.5703125000000000000, 0.5781250000000000000, 0.5859375000000000000, 0.5937500000000000000, 0.6015625000000000000, 0.6093750000000000000, 0.6171875000000000000, 0.6250000000000000000, 0.6328125000000000000, 0.6406250000000000000, 0.6484375000000000000, 0.6562500000000000000, 0.6640625000000000000, 0.6718750000000000000, 0.6796875000000000000, 0.6875000000000000000, 0.6953125000000000000, 0.7031250000000000000, 0.7109375000000000000, 0.7187500000000000000, 0.7265625000000000000, 0.7343750000000000000, 0.7421875000000000000, 0.7500000000000000000, 0.7578125000000000000, 0.7656250000000000000, 0.7734375000000000000, 0.7812500000000000000, 0.7890625000000000000, 0.7968750000000000000, 0.8046875000000000000, 0.8125000000000000000, 0.8203125000000000000, 0.8281250000000000000, 0.8359375000000000000, 0.8437500000000000000, 0.8515625000000000000, 0.8593750000000000000, 0.8671875000000000000, 0.8750000000000000000, 0.8828125000000000000, 0.8906250000000000000, 0.8984375000000000000, 0.9062500000000000000, 0.9140625000000000000, 0.9218750000000000000, 0.9296875000000000000, 0.9375000000000000000, 0.9453125000000000000, 0.9531250000000000000, 0.9609375000000000000, 0.9687500000000000000, 0.9765625000000000000, 0.9843750000000000000, 0.9921875000000000000, 1.000000000000000000 ),
 .UNSPECIFIED. ) ;
#2407 = CARTESIAN_POINT ( 'NONE',  ( -7.245889760505162869, 4.668767092638087313, 1.999999999999998224 ) ) ;
#2408 = CARTESIAN_POINT ( 'NONE',  ( 0.000000000000000000, 0.000000000000000000, -8.000000000000000000 ) ) ;
#2409 = CARTESIAN_POINT ( 'NONE',  ( -6.317162512443194267, 3.238855812894541941, 1.999999999999998224 ) ) ;
#2410 =( GEOMETRIC_REPRESENTATION_CONTEXT ( 3 ) GLOBAL_UNCERTAINTY_ASSIGNED_CONTEXT ( ( #1988 ) ) GLOBAL_UNIT_ASSIGNED_CONTEXT ( ( #3797, #2098, #3883 ) ) REPRESENTATION_CONTEXT ( 'NONE', 'WORKASPACE' ) );
#2411 = ORIENTED_EDGE ( 'NONE', *, *, #1421, .T. ) ;
#2412 = CARTESIAN_POINT ( 'NONE',  ( 5.053476174607396842, -5.757900651972986950, 1.999999999999998224 ) ) ;
#2413 = PLANE ( 'NONE',  #4479 ) ;
#2414 = LINE ( 'NONE', #1062, #3380 ) ;
#2415 = CARTESIAN_POINT ( 'NONE',  ( 9.320190601379009010, -2.164585516638707574, 1.999999999999998224 ) ) ;
#2416 = DIRECTION ( 'NONE',  ( -1.000000000000000000, 0.000000000000000000, 0.000000000000000000 ) ) ;
#2417 = CARTESIAN_POINT ( 'NONE',  ( 23.48484848484848442, -8.570991287109677614, -4.000000000000000000 ) ) ;
#2418 = ORIENTED_EDGE ( 'NONE', *, *, #5527, .T. ) ;
#2419 = CARTESIAN_POINT ( 'NONE',  ( 18.00000000000000000, 1.553654299240552096E-15, 16.41957833606399930 ) ) ;
#2420 = CYLINDRICAL_SURFACE ( 'NONE', #2900, 5.000000000000000000 ) ;
#2421 = CARTESIAN_POINT ( 'NONE',  ( 0.5754137710878161061, 8.770917875152035137, 1.999999999999998224 ) ) ;
#2422 = AXIS2_PLACEMENT_3D ( 'NONE', #4327, #3514, #2107 ) ;
#2423 = CARTESIAN_POINT ( 'NONE',  ( -2.153669193480074018, -8.035861145135083206, 13.99999999999999645 ) ) ;
#2424 = DIRECTION ( 'NONE',  ( 0.000000000000000000, 0.000000000000000000, -1.000000000000000000 ) ) ;
#2425 = EDGE_LOOP ( 'NONE', ( #3605, #1035, #602, #2829 ) ) ;
#2426 = PRODUCT_DEFINITION_SHAPE ( 'NONE', 'NONE',  #2040 ) ;
#2427 = DIRECTION ( 'NONE',  ( -0.9999273757268464236, 0.01205169166640771006, 2.722181309742254022E-20 ) ) ;
#2428 = ORIENTED_EDGE ( 'NONE', *, *, #2544, .T. ) ;
#2429 = CARTESIAN_POINT ( 'NONE',  ( 1.300000000000000044, -0.7216878364870319418, 1.249999999999999778 ) ) ;
#2430 = AXIS2_PLACEMENT_3D ( 'NONE', #3981, #3439, #5197 ) ;
#2431 = CARTESIAN_POINT ( 'NONE',  ( -6.734745854536168252, 2.161492950162117399, 14.00000000000000000 ) ) ;
#2432 = CARTESIAN_POINT ( 'NONE',  ( -8.411612136543094920, -4.319922787977579226, 13.99999999999999645 ) ) ;
#2433 = AXIS2_PLACEMENT_3D ( 'NONE', #5119, #3418, #5085 ) ;
#2434 = CARTESIAN_POINT ( 'NONE',  ( 3.173694703385745886, 5.505084763670784476, 14.00000000000000000 ) ) ;
#2435 = ORIENTED_EDGE ( 'NONE', *, *, #5235, .T. ) ;
#2436 = CARTESIAN_POINT ( 'NONE',  ( -1.592064345877699072, 9.625584969238365929, 1.999999999999998224 ) ) ;
#2437 = ADVANCED_FACE ( 'NONE', ( #1702 ), #3166, .T. ) ;
#2438 = FACE_BOUND ( 'NONE', #3207, .T. ) ;
#2439 =( NAMED_UNIT ( * ) SI_UNIT ( $, .STERADIAN. ) SOLID_ANGLE_UNIT ( ) );
#2440 = CARTESIAN_POINT ( 'NONE',  ( 4.290186206382708534, 5.996800006796977556, 1.999999999999998224 ) ) ;
#2441 = CIRCLE ( 'NONE', #4097, 23.00000000000000000 ) ;
#2442 = EDGE_CURVE ( 'NONE', #11, #2508, #4456, .T. ) ;
#2443 = ORIENTED_EDGE ( 'NONE', *, *, #2367, .F. ) ;
#2444 = CARTESIAN_POINT ( 'NONE',  ( -1.105557477332586247, -6.708264047591375956, 1.999999999999998224 ) ) ;
#2445 = CARTESIAN_POINT ( 'NONE',  ( -2.965071238690785371, 6.007415411094349622, 1.999999999999998224 ) ) ;
#2446 = CARTESIAN_POINT ( 'NONE',  ( -4.372214883940321428, 6.312905667202753257, 13.99999999999999645 ) ) ;
#2447 = VECTOR ( 'NONE', #116, 1000.000000000000000 ) ;
#2448 = CARTESIAN_POINT ( 'NONE',  ( 2.000000000000000000, 0.000000000000000000, 4.000000000000000000 ) ) ;
#2449 = PRESENTATION_LAYER_ASSIGNMENT (  '', '', ( #4931 ) ) ;
#2450 = FACE_OUTER_BOUND ( 'NONE', #2890, .T. ) ;
#2451 = ORIENTED_EDGE ( 'NONE', *, *, #1643, .T. ) ;
#2452 = CARTESIAN_POINT ( 'NONE',  ( 22.99999999999999645, -8.485281374238580199, -4.000000000000000000 ) ) ;
#2453 = CARTESIAN_POINT ( 'NONE',  ( 8.269507991092027055, 6.356934974246627235, 14.00000000000000000 ) ) ;
#2454 = CARTESIAN_POINT ( 'NONE',  ( -5.337360893037004672, -7.710592058383595848, 1.999999999999998224 ) ) ;
#2455 = ADVANCED_FACE ( 'NONE', ( #1242 ), #3004, .T. ) ;
#2456 = VECTOR ( 'NONE', #3756, 1000.000000000000114 ) ;
#2457 = CARTESIAN_POINT ( 'NONE',  ( 6.679452517770527287, -4.623421500472437273, 13.99999999999999645 ) ) ;
#2458 = PLANE ( 'NONE',  #1136 ) ;
#2459 = VERTEX_POINT ( 'NONE', #3862 ) ;
#2460 = LINE ( 'NONE', #5108, #1981 ) ;
#2461 = VERTEX_POINT ( 'NONE', #2133 ) ;
#2462 = AXIS2_PLACEMENT_3D ( 'NONE', #3769, #5206, #2960 ) ;
#2463 = CARTESIAN_POINT ( 'NONE',  ( 2.400000000000000799, 0.000000000000000000, 1.999999999999999112 ) ) ;
#2464 = CARTESIAN_POINT ( 'NONE',  ( 0.5542950790998155686, -6.736796398737816105, 14.00000000000000000 ) ) ;
#2465 = CARTESIAN_POINT ( 'NONE',  ( 8.993528569561179964, -4.616306094804236260, 13.99999999999999645 ) ) ;
#2466 = CARTESIAN_POINT ( 'NONE',  ( 2.690160903457257557, 6.823041841979409661, 14.00000000000000000 ) ) ;
#2467 = EDGE_LOOP ( 'NONE', ( #3465, #1416, #5107, #3219, #3354, #1592, #3519, #2569 ) ) ;
#2468 = CARTESIAN_POINT ( 'NONE',  ( -9.247353065533557626, -2.155497948345702408, 1.999999999999998224 ) ) ;
#2469 = CARTESIAN_POINT ( 'NONE',  ( 12.50000000000000000, 1.530808498934191521E-15, 14.00000000000000000 ) ) ;
#2470 = SURFACE_STYLE_FILL_AREA ( #5203 ) ;
#2471 = CARTESIAN_POINT ( 'NONE',  ( -6.667513054348624735, -4.302816426345351886, 1.999999999999998224 ) ) ;
#2472 = LINE ( 'NONE', #4205, #5311 ) ;
#2473 = EDGE_CURVE ( 'NONE', #534, #2009, #4820, .T. ) ;
#2474 = CARTESIAN_POINT ( 'NONE',  ( 5.887534416617372202, 3.663839002572494952, 13.99999999999999645 ) ) ;
#2475 = B_SPLINE_CURVE_WITH_KNOTS ( 'NONE', 3,
 ( #1377, #1746, #3133, #2233, #3905, #3517, #883, #1292, #4881, #423, #3501, #365, #4855, #3988, #3023, #5262, #1316, #3937, #854, #3077, #4822, #48, #2670, #2642, #4339, #1722, #3475, #938, #4396, #4421, #1773, #20, #2181, #2122, #451, #1687, #2210, #1803, #3559, #3444, #1261, #4315, #390, #5236, #3050, #3876, #3528, #4793, #4767, #3961, #2150, #5290, #5318, #1347, #828, #5202, #2580, #5661, #3106, #911, #4369, #969, #3750, #265, #1590, #997, #2024, #1832, #1401, #705, #4641, #3590, #4155, #5343, #1430, #2395, #3716, #506, #4049, #2263, #2885, #1962, #3294, #3350, #2727, #5507, #3778, #5103, #2756, #5534, #3163, #4909, #2457, #4215, #4478, #209, #538, #3189, #5476, #1537, #4020, #2859, #2423, #4185, #2692, #4448, #4940, #5042, #2289, #644, #77, #103, #1860, #3616, #5373, #4586, #1102, #4612, #671, #237, #1997, #1566, #3322, #5069, #1128, #3406, #5645, #839, #351, #4352, #4268, #4694, #1161, #2048, #2972, #3921, #406, #2165, #5134, #4779, #5615, #755, #4669, #730, #320, #3863, #3034, #2080, #1244, #3805, #3430, #2536, #4720, #2942, #3486, #4299, #5591, #4751, #2916, #5674, #3838, #5562, #2106, #1675, #783, #5158, #5185, #3005, #814, #1735, #2566, #4326, #1650, #2506, #2483, #1218, #375, #2136, #3890, #1704, #1621, #3458, #4239, #5222, #2594, #290, #3381, #1192, #1279, #4922, #5303, #4838, #1389, #5248, #2743, #2275, #1845, #115, #4063, #4004, #3601, #2194, #868, #4494, #3948, #61, #1819, #2710, #4462, #439, #89, #4035, #1364, #4804, #3120, #2221, #32, #2627, #1871, #1329, #462, #3146, #1304, #548, #5355, #1412, #3062, #4382, #3575, #3175, #487, #1786, #3092, #898, #983, #2302, #2655, #7, #3543, #3972, #1757, #3513 ),
 .UNSPECIFIED., .F., .F.,
 ( 4, 2, 2, 2, 2, 2, 2, 2, 2, 2, 2, 2, 2, 2, 2, 2, 2, 2, 2, 2, 2, 2, 2, 2, 2, 2, 2, 2, 2, 2, 2, 2, 2, 2, 2, 2, 2, 2, 2, 2, 2, 2, 2, 2, 2, 2, 2, 2, 2, 2, 2, 2, 2, 2, 2, 2, 2, 2, 2, 2, 2, 2, 2, 2, 2, 2, 2, 2, 2, 2, 2, 2, 2, 2, 2, 2, 2, 2, 2, 2, 2, 2, 2, 2, 2, 2, 2, 2, 2, 2, 2, 2, 2, 2, 2, 2, 2, 2, 2, 2, 2, 2, 2, 2, 2, 2, 2, 2, 2, 2, 2, 2, 2, 2, 2, 2, 2, 2, 2, 2, 4 ),
 ( 0.000000000000000000, 0.01562500000000000000, 0.03125000000000000000, 0.04687500000000000000, 0.06250000000000000000, 0.07812500000000000000, 0.09375000000000000000, 0.1093750000000000000, 0.1250000000000000000, 0.1328125000000000000, 0.1406250000000000000, 0.1484375000000000000, 0.1562500000000000000, 0.1640625000000000000, 0.1718750000000000000, 0.1796875000000000000, 0.1875000000000000000, 0.1953125000000000000, 0.2031250000000000000, 0.2109375000000000000, 0.2187500000000000000, 0.2265625000000000000, 0.2343750000000000000, 0.2421875000000000000, 0.2500000000000000000, 0.2578125000000000000, 0.2656250000000000000, 0.2734375000000000000, 0.2812500000000000000, 0.2890625000000000000, 0.2968750000000000000, 0.3046875000000000000, 0.3125000000000000000, 0.3203125000000000000, 0.3281250000000000000, 0.3359375000000000000, 0.3437500000000000000, 0.3515625000000000000, 0.3593750000000000000, 0.3671875000000000000, 0.3750000000000000000, 0.3828125000000000000, 0.3906250000000000000, 0.3984375000000000000, 0.4062500000000000000, 0.4140625000000000000, 0.4218750000000000000, 0.4296875000000000000, 0.4375000000000000000, 0.4453125000000000000, 0.4531250000000000000, 0.4609375000000000000, 0.4687500000000000000, 0.4765625000000000000, 0.4843750000000000000, 0.4921875000000000000, 0.5000000000000000000, 0.5078125000000000000, 0.5156250000000000000, 0.5234375000000000000, 0.5312500000000000000, 0.5390625000000000000, 0.5468750000000000000, 0.5546875000000000000, 0.5625000000000000000, 0.5703125000000000000, 0.5781250000000000000, 0.5859375000000000000, 0.5937500000000000000, 0.6015625000000000000, 0.6093750000000000000, 0.6171875000000000000, 0.6250000000000000000, 0.6328125000000000000, 0.6406250000000000000, 0.6484375000000000000, 0.6562500000000000000, 0.6640625000000000000, 0.6718750000000000000, 0.6796875000000000000, 0.6875000000000000000, 0.6953125000000000000, 0.7031250000000000000, 0.7109375000000000000, 0.7187500000000000000, 0.7265625000000000000, 0.7343750000000000000, 0.7421875000000000000, 0.7500000000000000000, 0.7578125000000000000, 0.7656250000000000000, 0.7734375000000000000, 0.7812500000000000000, 0.7890625000000000000, 0.7968750000000000000, 0.8046875000000000000, 0.8125000000000000000, 0.8203125000000000000, 0.8281250000000000000, 0.8359375000000000000, 0.8437500000000000000, 0.8515625000000000000, 0.8593750000000000000, 0.8671875000000000000, 0.8750000000000000000, 0.8828125000000000000, 0.8906250000000000000, 0.8984375000000000000, 0.9062500000000000000, 0.9140625000000000000, 0.9218750000000000000, 0.9296875000000000000, 0.9375000000000000000, 0.9453125000000000000, 0.9531250000000000000, 0.9609375000000000000, 0.9687500000000000000, 0.9765625000000000000, 0.9843750000000000000, 0.9921875000000000000, 1.000000000000000000 ),
 .UNSPECIFIED. ) ;
#2476 = PRESENTATION_STYLE_ASSIGNMENT (( #4742 ) ) ;
#2477 = DIRECTION ( 'NONE',  ( -1.000000000000000000, 0.000000000000000000, 0.000000000000000000 ) ) ;
#2478 = CARTESIAN_POINT ( 'NONE',  ( 5.000000000000000000, -6.123233995736766282E-16, -8.000000000000000000 ) ) ;
#2479 = ORIENTED_EDGE ( 'NONE', *, *, #2700, .T. ) ;
#2480 = DIRECTION ( 'NONE',  ( 1.000000000000000000, 0.000000000000000000, 0.000000000000000000 ) ) ;
#2481 = FACE_OUTER_BOUND ( 'NONE', #2838, .T. ) ;
#2482 = CARTESIAN_POINT ( 'NONE',  ( -8.745075223330342595, 3.959260399367897421, 1.999999999999998224 ) ) ;
#2483 = CARTESIAN_POINT ( 'NONE',  ( -3.127066335681350395, 9.214240776398044730, 13.99999999999999645 ) ) ;
#2484 = CARTESIAN_POINT ( 'NONE',  ( -8.332455577112462208, 5.761155596212925722, 14.00000000000000000 ) ) ;
#2485 = EDGE_CURVE ( 'NONE', #261, #660, #4914, .T. ) ;
#2486 = ORIENTED_EDGE ( 'NONE', *, *, #2306, .F. ) ;
#2487 = DIRECTION ( 'NONE',  ( -0.000000000000000000, 0.4999999999999998890, -0.8660254037844387076 ) ) ;
#2488 = ORIENTED_EDGE ( 'NONE', *, *, #4273, .F. ) ;
#2489 = DIRECTION ( 'NONE',  ( 1.000000000000000000, 0.000000000000000000, -0.000000000000000000 ) ) ;
#2490 = CARTESIAN_POINT ( 'NONE',  ( 3.520917041835319505, -6.848083076131263880, 14.00000000000000000 ) ) ;
#2491 = CARTESIAN_POINT ( 'NONE',  ( 1.954797901281673633, -9.037865403626287986, 13.99999999999999645 ) ) ;
#2492 = CARTESIAN_POINT ( 'NONE',  ( -4.089163901200158158, 5.898691170884823975, 14.00000000000000000 ) ) ;
#2493 = ORIENTED_EDGE ( 'NONE', *, *, #2950, .T. ) ;
#2494 = CARTESIAN_POINT ( 'NONE',  ( 7.233280636258586860, 6.778630567624379211, 1.999999999999998224 ) ) ;
#2495 = CARTESIAN_POINT ( 'NONE',  ( 2.369394374793902802, -7.353877281245869035, 1.999999999999998224 ) ) ;
#2496 = CARTESIAN_POINT ( 'NONE',  ( 0.000000000000000000, 0.000000000000000000, -58.22539674441618018 ) ) ;
#2497 = CARTESIAN_POINT ( 'NONE',  ( -2.919577271296576182, -6.733962781534541975, 13.99999999999999645 ) ) ;
#2498 =( GEOMETRIC_REPRESENTATION_CONTEXT ( 3 ) GLOBAL_UNCERTAINTY_ASSIGNED_CONTEXT ( ( #3112 ) ) GLOBAL_UNIT_ASSIGNED_CONTEXT ( ( #3372, #3829, #3140 ) ) REPRESENTATION_CONTEXT ( 'NONE', 'WORKASPACE' ) );
#2499 = CARTESIAN_POINT ( 'NONE',  ( 9.522148329495122354, -0.6196525284525815636, 1.999999999999998224 ) ) ;
#2500 = DIRECTION ( 'NONE',  ( -3.540989467475305966E-16, -1.000000000000000000, -0.000000000000000000 ) ) ;
#2501 = CARTESIAN_POINT ( 'NONE',  ( 0.000000000000000000, 0.000000000000000000, -8.000000000000000000 ) ) ;
#2502 = ORIENTED_EDGE ( 'NONE', *, *, #4759, .F. ) ;
#2503 = CARTESIAN_POINT ( 'NONE',  ( 0.000000000000000000, 0.000000000000000000, 4.000000000000000000 ) ) ;
#2504 = PRODUCT_DEFINITION_FORMATION_WITH_SPECIFIED_SOURCE ( 'ANY', '', #2846, .NOT_KNOWN. ) ;
#2505 = FACE_OUTER_BOUND ( 'NONE', #3224, .T. ) ;
#2506 = CARTESIAN_POINT ( 'NONE',  ( -3.867583043141954224, 8.914321633329153727, 13.99999999999999645 ) ) ;
#2507 = CARTESIAN_POINT ( 'NONE',  ( -7.304208470128496167, 7.056621303512280896, 14.00000000000000000 ) ) ;
#2508 = VERTEX_POINT ( 'NONE', #350 ) ;
#2509 = PLANE ( 'NONE',  #701 ) ;
#2510 = ORIENTED_EDGE ( 'NONE', *, *, #2804, .T. ) ;
#2511 = CARTESIAN_POINT ( 'NONE',  ( 1.300000000000000044, 0.000000000000000000, 0.000000000000000000 ) ) ;
#2512 = CARTESIAN_POINT ( 'NONE',  ( -3.715337444063475658, -5.771435016728993617, 14.00000000000000000 ) ) ;
#2513 = CARTESIAN_POINT ( 'NONE',  ( -10.42442484909544653, -1.371544430045602558, 13.99999999999999645 ) ) ;
#2514 = CIRCLE ( 'NONE', #5369, 1.249999999999999778 ) ;
#2515 = CARTESIAN_POINT ( 'NONE',  ( 5.195030181282107584, -4.117271336869512410, 14.00000000000000000 ) ) ;
#2516 =( GEOMETRIC_REPRESENTATION_CONTEXT ( 3 ) GLOBAL_UNCERTAINTY_ASSIGNED_CONTEXT ( ( #2301 ) ) GLOBAL_UNIT_ASSIGNED_CONTEXT ( ( #4064, #3577, #3148 ) ) REPRESENTATION_CONTEXT ( 'NONE', 'WORKASPACE' ) );
#2517 = VERTEX_POINT ( 'NONE', #2268 ) ;
#2518 = CARTESIAN_POINT ( 'NONE',  ( -7.080399483669990168, -6.208478756603781790, 1.999999999999998224 ) ) ;
#2519 = VECTOR ( 'NONE', #1230, 1000.000000000000000 ) ;
#2520 = CARTESIAN_POINT ( 'NONE',  ( 0.000000000000000000, 0.000000000000000000, 8.000000000000000000 ) ) ;
#2521 = CARTESIAN_POINT ( 'NONE',  ( 4.415008247871750058, 7.106745273741266189, 1.999999999999998224 ) ) ;
#2522 = EDGE_CURVE ( 'NONE', #4842, #4044, #4749, .T. ) ;
#2523 = VECTOR ( 'NONE', #4234, 1000.000000000000114 ) ;
#2524 = MECHANICAL_DESIGN_GEOMETRIC_PRESENTATION_REPRESENTATION (  '', ( #5004 ), #4279 ) ;
#2525 = CARTESIAN_POINT ( 'NONE',  ( 5.806279480217827249, -1.975834710110474512, 1.999999999999998224 ) ) ;
#2526 = CARTESIAN_POINT ( 'NONE',  ( 2.406079317367887604, 6.392288322179703108, 13.99999999999999645 ) ) ;
#2527 = VECTOR ( 'NONE', #3463, 1000.000000000000000 ) ;
#2528 = CARTESIAN_POINT ( 'NONE',  ( 5.519166806814063797, -7.959527472085689226, 1.999999999999998224 ) ) ;
#2529 = EDGE_CURVE ( 'NONE', #3158, #4137, #5642, .T. ) ;
#2530 = LINE ( 'NONE', #1213, #4738 ) ;
#2531 = DIRECTION ( 'NONE',  ( -0.000000000000000000, -0.000000000000000000, 1.000000000000000000 ) ) ;
#2532 = ORIENTED_EDGE ( 'NONE', *, *, #1973, .T. ) ;
#2533 = FACE_OUTER_BOUND ( 'NONE', #1738, .T. ) ;
#2534 = CARTESIAN_POINT ( 'NONE',  ( 1.300000000000000044, 0.000000000000000000, 0.000000000000000000 ) ) ;
#2535 = EDGE_CURVE ( 'NONE', #36, #726, #2105, .T. ) ;
#2536 = CARTESIAN_POINT ( 'NONE',  ( -0.3010823416051303103, -9.281161307073869438, 13.99999999999999645 ) ) ;
#2537 = CLOSED_SHELL ( 'NONE', ( #5675, #1435, #3259, #3997, #1795, #5533, #5063, #5017, #5428, #4827, #5266, #1467, #2995, #2663, #488, #154, #4509, #4025, #1935, #4146, #2588, #3195, #5328, #3909, #3154, #3661 ) ) ;
#2538 = FACE_OUTER_BOUND ( 'NONE', #3489, .T. ) ;
#2539 = EDGE_LOOP ( 'NONE', ( #4970, #3860 ) ) ;
#2540 = DIRECTION ( 'NONE',  ( -0.000000000000000000, -0.4999999999999999445, -0.8660254037844387076 ) ) ;
#2541 = ORIENTED_EDGE ( 'NONE', *, *, #1149, .F. ) ;
#2542 = CARTESIAN_POINT ( 'NONE',  ( 1.500000000000002887, 24.95495942693556302, 1.371299631966804711 ) ) ;
#2543 = CARTESIAN_POINT ( 'NONE',  ( 7.925371078819432036, 2.990572132494779378, 14.00000000000000000 ) ) ;
#2544 = EDGE_CURVE ( 'NONE', #4159, #4295, #5196, .T. ) ;
#2545 = CARTESIAN_POINT ( 'NONE',  ( 4.914575889516862972, -3.754581871930560144, 1.999999999999998224 ) ) ;
#2546 = CLOSED_SHELL ( 'NONE', ( #764, #3249, #5603, #1844, #3057, #3313, #998, #2288 ) ) ;
#2547 = CIRCLE ( 'NONE', #4016, 1.249999999999999778 ) ;
#2548 = DIRECTION ( 'NONE',  ( 0.000000000000000000, 0.000000000000000000, -1.000000000000000000 ) ) ;
#2549 = CARTESIAN_POINT ( 'NONE',  ( -7.019001384594682591, 0.4577903460187995877, 14.00000000000000000 ) ) ;
#2550 = CIRCLE ( 'NONE', #2271, 22.50000000000000355 ) ;
#2551 = ORIENTED_EDGE ( 'NONE', *, *, #925, .F. ) ;
#2552 = CARTESIAN_POINT ( 'NONE',  ( -5.337360893037004672, -7.710592058383595848, 1.999999999999998224 ) ) ;
#2553 = AXIS2_PLACEMENT_3D ( 'NONE', #2286, #5021, #4506 ) ;
#2554 = DIRECTION ( 'NONE',  ( 1.000000000000000000, 0.000000000000000000, 0.000000000000000000 ) ) ;
#2555 = CARTESIAN_POINT ( 'NONE',  ( 0.000000000000000000, 0.000000000000000000, 16.00000000000000000 ) ) ;
#2556 = CARTESIAN_POINT ( 'NONE',  ( 7.320916985966518631, 1.587212364775676843, 1.999999999999998224 ) ) ;
#2557 = EDGE_CURVE ( 'NONE', #2855, #2946, #4860, .T. ) ;
#2558 = CARTESIAN_POINT ( 'NONE',  ( -4.310533329768688304, 5.077046166951620698, 1.999999999999412914 ) ) ;
#2559 = CARTESIAN_POINT ( 'NONE',  ( -5.978927507574435474, 2.933119789328458182, 13.99999999999999645 ) ) ;
#2560 = CARTESIAN_POINT ( 'NONE',  ( 0.1634456542307745064, 10.28566380800474533, 1.999999999999998224 ) ) ;
#2561 = LINE ( 'NONE', #809, #147 ) ;
#2562 = CARTESIAN_POINT ( 'NONE',  ( 1.300000000000000044, -0.7216878364870319418, 1.249999999999999778 ) ) ;
#2563 = EDGE_LOOP ( 'NONE', ( #3144, #4724, #5059, #1088 ) ) ;
#2564 = CARTESIAN_POINT ( 'NONE',  ( 0.000000000000000000, 0.000000000000000000, 4.000000000000000000 ) ) ;
#2565 = CARTESIAN_POINT ( 'NONE',  ( 17.99999999999999289, -15.01665741768121443, -8.000000000000000000 ) ) ;
#2566 = CARTESIAN_POINT ( 'NONE',  ( -7.044187934146358465, 6.598551529630926282, 13.99999999999999645 ) ) ;
#2567 = EDGE_CURVE ( 'NONE', #4270, #2946, #2714, .T. ) ;
#2568 = DIRECTION ( 'NONE',  ( -0.000000000000000000, -0.000000000000000000, 1.000000000000000000 ) ) ;
#2569 = ORIENTED_EDGE ( 'NONE', *, *, #2896, .F. ) ;
#2570 = CARTESIAN_POINT ( 'NONE',  ( 5.000000000000001776, 24.49489742783178414, 4.000000000000000000 ) ) ;
#2571 = ORIENTED_EDGE ( 'NONE', *, *, #3073, .F. ) ;
#2572 = DIRECTION ( 'NONE',  ( -0.000000000000000000, 1.000000000000000000, 1.224646799147353207E-16 ) ) ;
#2573 = CARTESIAN_POINT ( 'NONE',  ( -6.826495404309340209, 4.393449859560456083, 14.00000000000000000 ) ) ;
#2574 = CARTESIAN_POINT ( 'NONE',  ( -7.035243215357270152, 8.023489478516461659, 13.99999999999999645 ) ) ;
#2575 = PRODUCT_DEFINITION_CONTEXT ( 'detailed design', #2102, 'design' ) ;
#2576 = DIRECTION ( 'NONE',  ( -0.000000000000000000, 1.000000000000000000, 0.000000000000000000 ) ) ;
#2577 = CARTESIAN_POINT ( 'NONE',  ( -6.826495404309340209, 4.393449859560456083, 14.00000000000000000 ) ) ;
#2578 = ORIENTED_EDGE ( 'NONE', *, *, #1697, .F. ) ;
#2579 = CARTESIAN_POINT ( 'NONE',  ( 7.456063200420987691, 7.959410280423138140, 1.999999999999998224 ) ) ;
#2580 = CARTESIAN_POINT ( 'NONE',  ( -5.810612947750823487, -4.611264106266947493, 13.99999999999999645 ) ) ;
#2581 = APPLICATION_PROTOCOL_DEFINITION ( 'draft international standard', 'automotive_design', 1998, #5525 ) ;
#2582 = CARTESIAN_POINT ( 'NONE',  ( -6.185289998984973003, -6.402116997106289453, 1.999999999999998224 ) ) ;
#2583 = CARTESIAN_POINT ( 'NONE',  ( -0.5931392160223127874, -7.263020831007572120, 1.999999999999998224 ) ) ;
#2584 = CARTESIAN_POINT ( 'NONE',  ( 8.164254108709979363, -4.026826083952141921, 13.99999999999999645 ) ) ;
#2585 = MANIFOLD_SOLID_BREP ( 'Sweep1', #510 ) ;
#2586 = DIRECTION ( 'NONE',  ( 0.000000000000000000, 0.000000000000000000, -1.000000000000000000 ) ) ;
#2587 = CARTESIAN_POINT ( 'NONE',  ( 1.124407659250306279, -9.699258357302506184, 1.999999999999998224 ) ) ;
#2588 = ADVANCED_FACE ( 'NONE', ( #5378 ), #4425, .F. ) ;
#2589 = DIRECTION ( 'NONE',  ( 0.000000000000000000, 0.000000000000000000, 1.000000000000000000 ) ) ;
#2590 = CARTESIAN_POINT ( 'NONE',  ( 1.300000000000000044, 0.7216878364870328300, 1.249999999999999778 ) ) ;
#2591 = EDGE_LOOP ( 'NONE', ( #65, #2244, #3892, #5539 ) ) ;
#2592 = CARTESIAN_POINT ( 'NONE',  ( 2.021687836487040535, 2.168404344971008868E-16, 0.000000000000000000 ) ) ;
#2593 = COLOUR_RGB ( '',0.8941176470588234615, 0.8941176470588234615, 0.8941176470588234615 ) ;
#2594 = CARTESIAN_POINT ( 'NONE',  ( 7.775655769254120386, 6.170250810330326630, 13.99999999999999645 ) ) ;
#2595 = MANIFOLD_SOLID_BREP ( '<outer cover 1>-<Fillet1>', #2537 ) ;
#2596 = CARTESIAN_POINT ( 'NONE',  ( 18.00000000000000000, 1.553654299240552096E-15, -4.000000000000000000 ) ) ;
#2597 = VERTEX_POINT ( 'NONE', #2937 ) ;
#2598 = DIRECTION ( 'NONE',  ( -0.000000000000000000, -0.000000000000000000, -1.000000000000000000 ) ) ;
#2599 = ORIENTED_EDGE ( 'NONE', *, *, #2389, .F. ) ;
#2600 = LINE ( 'NONE', #2947, #3469 ) ;
#2601 = CARTESIAN_POINT ( 'NONE',  ( -5.581220830679986200, 5.949058968288507110, 14.00000000000000000 ) ) ;
#2602 = CARTESIAN_POINT ( 'NONE',  ( -1.424809953814531127, 6.586142414399820844, 1.999999999999998224 ) ) ;
#2603 = EDGE_CURVE ( 'NONE', #4992, #354, #5217, .T. ) ;
#2604 = DIRECTION ( 'NONE',  ( 1.000000000000000000, 0.000000000000000000, 0.000000000000000000 ) ) ;
#2605 = CARTESIAN_POINT ( 'NONE',  ( 3.810368753942760200, 7.433568398487740758, 14.00000000000000000 ) ) ;
#2606 = ORIENTED_EDGE ( 'NONE', *, *, #2473, .F. ) ;
#2607 = CIRCLE ( 'NONE', #2422, 23.00000000000000000 ) ;
#2608 = DIRECTION ( 'NONE',  ( -0.000000000000000000, -0.000000000000000000, 1.000000000000000000 ) ) ;
#2609 = DIRECTION ( 'NONE',  ( -1.156482317317871725E-16, -1.000000000000000000, 0.000000000000000000 ) ) ;
#2610 = CIRCLE ( 'NONE', #2892, 23.00000000000000000 ) ;
#2611 = SHAPE_DEFINITION_REPRESENTATION ( #269, #4116 ) ;
#2612 = CARTESIAN_POINT ( 'NONE',  ( 9.527640065893086430, 0.1642265212908741445, 1.999999999999998224 ) ) ;
#2613 = CARTESIAN_POINT ( 'NONE',  ( 7.409328306158467825, 2.927536720054290775, 1.999999999999998224 ) ) ;
#2614 = CARTESIAN_POINT ( 'NONE',  ( 7.132151089625189400, 3.519983721611798622, 13.99999999999999645 ) ) ;
#2615 = VECTOR ( 'NONE', #5323, 1000.000000000000000 ) ;
#2616 = ADVANCED_FACE ( 'NONE', ( #3375 ), #5129, .T. ) ;
#2617 = CARTESIAN_POINT ( 'NONE',  ( 23.48484848484848442, -8.570991287109677614, 8.000000000000000000 ) ) ;
#2618 = ADVANCED_FACE ( 'NONE', ( #4322 ), #2130, .T. ) ;
#2619 = PRODUCT_DEFINITION_SHAPE ( 'NONE', 'NONE',  #5691 ) ;
#2620 = CARTESIAN_POINT ( 'NONE',  ( -5.000000000000000000, 4.999999999999978684, -5.000000000000000000 ) ) ;
#2621 = AXIS2_PLACEMENT_3D ( 'NONE', #1276, #4297, #479 ) ;
#2622 = AXIS2_PLACEMENT_3D ( 'NONE', #5413, #4123, #4605 ) ;
#2623 = CARTESIAN_POINT ( 'NONE',  ( 3.896371052708264227, -4.167854722424304548, 1.999999999999998224 ) ) ;
#2624 = DIRECTION ( 'NONE',  ( 1.000000000000000000, 0.000000000000000000, 0.000000000000000000 ) ) ;
#2625 = ORIENTED_EDGE ( 'NONE', *, *, #1245, .F. ) ;
#2626 = MECHANICAL_DESIGN_GEOMETRIC_PRESENTATION_REPRESENTATION (  '', ( #1053 ), #47 ) ;
#2627 = CARTESIAN_POINT ( 'NONE',  ( -10.17357856257779680, 2.902115915870757679, 13.99999999999999645 ) ) ;
#2629 = ORIENTED_EDGE ( 'NONE', *, *, #1191, .F. ) ;
#2628 = AXIS2_PLACEMENT_3D ( 'NONE', #3037, #324, #5679 ) ;
#2630 = DIRECTION ( 'NONE',  ( -1.000000000000000000, 0.000000000000000000, 0.000000000000000000 ) ) ;
#2631 = ORIENTED_EDGE ( 'NONE', *, *, #4413, .T. ) ;
#2632 = EDGE_CURVE ( 'NONE', #2855, #899, #2805, .T. ) ;
#2633 = ORIENTED_EDGE ( 'NONE', *, *, #3973, .T. ) ;
#2634 = CARTESIAN_POINT ( 'NONE',  ( -7.963215149404076598, -4.094909132697305054, 14.00000000000000000 ) ) ;
#2635 = CARTESIAN_POINT ( 'NONE',  ( -0.4015567206217142693, -6.330257989742454683, 1.999999999999998224 ) ) ;
#2636 = AXIS2_PLACEMENT_3D ( 'NONE', #2797, #4547, #3685 ) ;
#2637 = PLANE ( 'NONE',  #5644 ) ;
#2638 = CARTESIAN_POINT ( 'NONE',  ( -2.020383375745357313, -7.552201994671271734, 14.00000000000000000 ) ) ;
#2639 = ORIENTED_EDGE ( 'NONE', *, *, #1421, .F. ) ;
#2640 = AXIS2_PLACEMENT_3D ( 'NONE', #3946, #2274, #1784 ) ;
#2641 = CARTESIAN_POINT ( 'NONE',  ( 5.279590631141700463, 9.498297537454860162, 1.999999999999998224 ) ) ;
#2642 = CARTESIAN_POINT ( 'NONE',  ( 0.2194671214740386012, 6.774136816532214667, 13.99999999999999645 ) ) ;
#2643 = AXIS2_PLACEMENT_3D ( 'NONE', #3435, #413, #790 ) ;
#2644 = APPLICATION_PROTOCOL_DEFINITION ( 'draft international standard', 'automotive_design', 1998, #1998 ) ;
#2645 = CARTESIAN_POINT ( 'NONE',  ( 8.370269057507494281, -1.803949267857694716, 1.999999999999998224 ) ) ;
#2646 = EDGE_CURVE ( 'NONE', #286, #1931, #1186, .T. ) ;
#2647 = CARTESIAN_POINT ( 'NONE',  ( -2.122668041763332347, 7.434468402752582250, 1.999999999999998224 ) ) ;
#2648 = VECTOR ( 'NONE', #1814, 1000.000000000000000 ) ;
#2649 = LINE ( 'NONE', #3994, #3993 ) ;
#2650 = LINE ( 'NONE', #5243, #121 ) ;
#2651 = CARTESIAN_POINT ( 'NONE',  ( 0.000000000000000000, 0.000000000000000000, -4.000000000000000000 ) ) ;
#2652 = CARTESIAN_POINT ( 'NONE',  ( 23.00000000000000000, -2.168404344971008868E-16, -8.000000000000000000 ) ) ;
#2653 = ORIENTED_EDGE ( 'NONE', *, *, #2300, .T. ) ;
#2654 = CARTESIAN_POINT ( 'NONE',  ( 22.50000000000000355, 2.755455298081545172E-15, 2.000000000000000000 ) ) ;
#2655 = CARTESIAN_POINT ( 'NONE',  ( 9.199536834907137361, 5.930433524308741156, 13.99999999999999645 ) ) ;
#2656 = DIRECTION ( 'NONE',  ( 0.000000000000000000, 0.8660254037844387076, -0.4999999999999999445 ) ) ;
#2657 = CARTESIAN_POINT ( 'NONE',  ( 6.000000000000001776, 0.000000000000000000, 13.99999999999999645 ) ) ;
#2658 = ORIENTED_EDGE ( 'NONE', *, *, #1888, .T. ) ;
#2659 = ORIENTED_EDGE ( 'NONE', *, *, #3049, .F. ) ;
#2660 = CARTESIAN_POINT ( 'NONE',  ( 7.311638624438943523, 4.225618826270838291, 14.00000000000000000 ) ) ;
#2661 = CARTESIAN_POINT ( 'NONE',  ( 1.015216742983932274, 7.730330528320553896, 1.999999999999998224 ) ) ;
#2662 = APPLICATION_CONTEXT ( 'automotive_design' ) ;
#2663 = ADVANCED_FACE ( 'NONE', ( #750 ), #1154, .T. ) ;
#2664 = DIRECTION ( 'NONE',  ( 0.000000000000000000, 0.000000000000000000, 1.000000000000000000 ) ) ;
#2665 = CARTESIAN_POINT ( 'NONE',  ( 1.147089839255721166, -8.682979827542890661, 14.00000000000000000 ) ) ;
#2666 = ORIENTED_EDGE ( 'NONE', *, *, #267, .T. ) ;
#2667 = CARTESIAN_POINT ( 'NONE',  ( 10.02239396097947655, -0.6576683464576721372, 1.999999999999998224 ) ) ;
#2668 = CARTESIAN_POINT ( 'NONE',  ( 0.1774200004017884857, 10.78715707688374614, 1.999999999999998224 ) ) ;
#2669 = UNCERTAINTY_MEASURE_WITH_UNIT (LENGTH_MEASURE( 1.000000000000000082E-05 ), #946, 'distance_accuracy_value', 'NONE');
#2670 = CARTESIAN_POINT ( 'NONE',  ( -0.8811140424828162176, 6.693995663234412419, 13.99999999999999645 ) ) ;
#2671 = CARTESIAN_POINT ( 'NONE',  ( 5.519166806814063797, -7.959527472085689226, 1.999999999999998224 ) ) ;
#2672 = CARTESIAN_POINT ( 'NONE',  ( 3.909482108038854431, 5.648312977191785045, 1.999999999999998224 ) ) ;
#2673 = DIRECTION ( 'NONE',  ( 1.000000000000000000, 0.000000000000000000, 0.000000000000000000 ) ) ;
#2674 = LINE ( 'NONE', #860, #3441 ) ;
#2675 = FACE_OUTER_BOUND ( 'NONE', #5511, .T. ) ;
#2676 = CARTESIAN_POINT ( 'NONE',  ( 4.815977876496239318, 4.225366587634176163, 1.999999999999998224 ) ) ;
#2677 = DIRECTION ( 'NONE',  ( -0.000000000000000000, -0.000000000000000000, 1.000000000000000000 ) ) ;
#2678 = ORIENTED_EDGE ( 'NONE', *, *, #1973, .F. ) ;
#2679 = CYLINDRICAL_SURFACE ( 'NONE', #867, 2.149999999999998579 ) ;
#2680 = CARTESIAN_POINT ( 'NONE',  ( 23.00000000000000000, -2.168404344971008868E-16, 16.41957833606399930 ) ) ;
#2681 = DIRECTION ( 'NONE',  ( -1.000000000000000000, -0.000000000000000000, -0.000000000000000000 ) ) ;
#2682 = ORIENTED_EDGE ( 'NONE', *, *, #3286, .F. ) ;
#2683 = ORIENTED_EDGE ( 'NONE', *, *, #3291, .F. ) ;
#2684 = CARTESIAN_POINT ( 'NONE',  ( -8.290222237439158093, 3.747600907060152586, 14.00000000000000000 ) ) ;
#2685 = CARTESIAN_POINT ( 'NONE',  ( 8.027649061863494140, -0.2602747315786821392, 1.999999999999998224 ) ) ;
#2686 = CARTESIAN_POINT ( 'NONE',  ( 8.518575158373787204, 0.2826087140540892162, 1.999999999999998224 ) ) ;
#2687 = CARTESIAN_POINT ( 'NONE',  ( -7.301858691287087311, -3.172613069824385956, 14.00000000000000000 ) ) ;
#2688 = ORIENTED_EDGE ( 'NONE', *, *, #2632, .T. ) ;
#2689 = CARTESIAN_POINT ( 'NONE',  ( -5.893815055328603947, 7.676334994785346311, 1.999999999999998224 ) ) ;
#2690 = CARTESIAN_POINT ( 'NONE',  ( 10.98697916625148707, 0.8999353979983775176, 1.999999999999998224 ) ) ;
#2691 =( REPRESENTATION_RELATIONSHIP ('NONE','NONE', #4854, #5261 ) REPRESENTATION_RELATIONSHIP_WITH_TRANSFORMATION ( #912 )SHAPE_REPRESENTATION_RELATIONSHIP( ) );
#2692 = CARTESIAN_POINT ( 'NONE',  ( -4.060726170632903198, -7.305992298388080286, 13.99999999999999645 ) ) ;
#2693 = PRODUCT_CONTEXT ( 'NONE', #5525, 'mechanical' ) ;
#2694 = CARTESIAN_POINT ( 'NONE',  ( 1.853537052132013363, -8.546502713975391075, 1.999999999999998224 ) ) ;
#2695 = ORIENTED_EDGE ( 'NONE', *, *, #1636, .F. ) ;
#2696 = CARTESIAN_POINT ( 'NONE',  ( 1.649120185255090298, 7.633850905136056575, 1.999999999999998224 ) ) ;
#2697 = SURFACE_STYLE_USAGE ( .BOTH. , #5322 ) ;
#2698 = COLOUR_RGB ( '',0.8941176470588234615, 0.8941176470588234615, 0.8941176470588234615 ) ;
#2699 = DIRECTION ( 'NONE',  ( -1.000000000000000000, 0.000000000000000000, 0.000000000000000000 ) ) ;
#2700 = EDGE_CURVE ( 'NONE', #2140, #3849, #5610, .T. ) ;
#2701 =( NAMED_UNIT ( * ) SI_UNIT ( $, .STERADIAN. ) SOLID_ANGLE_UNIT ( ) );
#2702 = CARTESIAN_POINT ( 'NONE',  ( 0.000000000000000000, 0.000000000000000000, 8.000000000000000000 ) ) ;
#2703 = CARTESIAN_POINT ( 'NONE',  ( 4.513069810084762601, -3.445129632735342451, 1.999999999999998224 ) ) ;
#2704 = AXIS2_PLACEMENT_3D ( 'NONE', #3932, #2145, #1683 ) ;
#2705 = CARTESIAN_POINT ( 'NONE',  ( 2.200000000000000622, 2.694222958124176020E-16, -2.199999999999999289 ) ) ;
#2706 = EDGE_LOOP ( 'NONE', ( #563, #1187, #139, #880 ) ) ;
#2707 = CARTESIAN_POINT ( 'NONE',  ( -1.380000000000054960, 3.291637795666119257E-15, 15.94994774640597512 ) ) ;
#2708 = UNCERTAINTY_MEASURE_WITH_UNIT (LENGTH_MEASURE( 1.000000000000000082E-05 ), #5247, 'distance_accuracy_value', 'NONE');
#2709 = CIRCLE ( 'NONE', #130, 5.000000000000000000 ) ;
#2710 = CARTESIAN_POINT ( 'NONE',  ( -6.045729098460493667, -8.441868823237593134, 13.99999999999999645 ) ) ;
#2711 = DIRECTION ( 'NONE',  ( 0.000000000000000000, 0.000000000000000000, 1.000000000000000000 ) ) ;
#2712 = LINE ( 'NONE', #1847, #2447 ) ;
#2713 = VERTEX_POINT ( 'NONE', #371 ) ;
#2714 = CIRCLE ( 'NONE', #134, 25.00000000000000000 ) ;
#2715 = ORIENTED_EDGE ( 'NONE', *, *, #3132, .F. ) ;
#2716 = CARTESIAN_POINT ( 'NONE',  ( -9.986481889892992569, 1.144076113142371787, 14.00000000000000000 ) ) ;
#2717 = CARTESIAN_POINT ( 'NONE',  ( 6.638644669766898154, 2.135480210976827387, 1.999999999999998224 ) ) ;
#2718 = AXIS2_PLACEMENT_3D ( 'NONE', #4783, #1737, #5161 ) ;
#2719 = CARTESIAN_POINT ( 'NONE',  ( 0.5385325299235221852, 8.270587056550796845, 1.999999999999998224 ) ) ;
#2720 = CARTESIAN_POINT ( 'NONE',  ( 9.164356920906893578, 2.464151434935829332, 14.00000000000000000 ) ) ;
#2721 = EDGE_CURVE ( 'NONE', #4627, #5308, #2967, .T. ) ;
#2722 = ORIENTED_EDGE ( 'NONE', *, *, #4565, .T. ) ;
#2723 = CARTESIAN_POINT ( 'NONE',  ( -5.651290410005069376, 9.082320918485367045, 1.999999999999998224 ) ) ;
#2724 = CARTESIAN_POINT ( 'NONE',  ( 6.315449825284095375, 1.474116854620425299, 14.00000000000000000 ) ) ;
#2725 = CARTESIAN_POINT ( 'NONE',  ( -8.440272934376814362, 1.393994921405934173, 13.99999999999999645 ) ) ;
#2726 = CIRCLE ( 'NONE', #1438, 0.2000000000000000944 ) ;
#2727 = CARTESIAN_POINT ( 'NONE',  ( 7.409328306158469601, 2.927536720054149555, 13.99999999999999645 ) ) ;
#2728 = CARTESIAN_POINT ( 'NONE',  ( -1.336592501075063666, -5.709464570123372162, 14.00000000000000000 ) ) ;
#2729 = AXIS2_PLACEMENT_3D ( 'NONE', #287, #2078, #3835 ) ;
#2730 = EDGE_CURVE ( 'NONE', #5595, #132, #779, .T. ) ;
#2731 = CARTESIAN_POINT ( 'NONE',  ( 5.381714297850622053, -6.137309488907494170, 1.999999999999998224 ) ) ;
#2732 = CARTESIAN_POINT ( 'NONE',  ( 1.300000000000000044, 1.443375672974065216, 7.017607234860990640E-28 ) ) ;
#2733 = CIRCLE ( 'NONE', #5304, 23.00000000000000000 ) ;
#2734 = CARTESIAN_POINT ( 'NONE',  ( 22.99999999999999645, -8.485281374238580199, 8.000000000000000000 ) ) ;
#2735 = SHAPE_REPRESENTATION_RELATIONSHIP ( 'NONE' , 'NONE' ,  #143, #694 ) ;
#2736 = DIRECTION ( 'NONE',  ( -4.364351673553916694E-15, 1.000000000000000000, 0.000000000000000000 ) ) ;
#2737 = ADVANCED_FACE ( 'NONE', ( #3799 ), #1239, .T. ) ;
#2738 = EDGE_LOOP ( 'NONE', ( #4379, #5404, #5162, #3648, #1521, #411, #3808, #4125, #1660 ) ) ;
#2739 = CIRCLE ( 'NONE', #625, 12.50000000000000000 ) ;
#2740 = CARTESIAN_POINT ( 'NONE',  ( -6.069783318623453106, -0.2142533344232669390, 1.999999999999998224 ) ) ;
#2741 = DIRECTION ( 'NONE',  ( 1.000000000000000000, 0.000000000000000000, 0.000000000000000000 ) ) ;
#2742 = DIRECTION ( 'NONE',  ( -1.000000000000000000, -0.000000000000000000, -0.000000000000000000 ) ) ;
#2743 = CARTESIAN_POINT ( 'NONE',  ( 8.595497693524210447, -5.345940745659388149, 13.99999999999999645 ) ) ;
#2744 = CARTESIAN_POINT ( 'NONE',  ( 0.000000000000000000, 0.000000000000000000, 2.000000000000000000 ) ) ;
#2745 = CARTESIAN_POINT ( 'NONE',  ( 17.99999999999999289, -15.01665741768121443, 4.000000000000000000 ) ) ;
#2746 = VERTEX_POINT ( 'NONE', #347 ) ;
#2747 = EDGE_LOOP ( 'NONE', ( #3352, #3950, #4438, #4650, #4225, #315 ) ) ;
#2748 = CARTESIAN_POINT ( 'NONE',  ( 9.522148329495834673, -0.6196525284526704924, 14.00000000000000000 ) ) ;
#2749 = CARTESIAN_POINT ( 'NONE',  ( -5.745624475482103755, 5.035517847229626476, 1.999999999999998224 ) ) ;
#2750 = CARTESIAN_POINT ( 'NONE',  ( -8.547479018124427341, -2.754496926847987748, 1.999999999999998224 ) ) ;
#2751 = CARTESIAN_POINT ( 'NONE',  ( 1.124407659250215685, -9.699258357303232714, 14.00000000000000000 ) ) ;
#2752 = ORIENTED_EDGE ( 'NONE', *, *, #559, .F. ) ;
#2753 = CARTESIAN_POINT ( 'NONE',  ( -7.660583958272733973, 7.409732212660907535, 1.999999999999998224 ) ) ;
#2754 = CARTESIAN_POINT ( 'NONE',  ( 5.400000000000002132, 26.45448922205832432, 24.08672805191341482 ) ) ;
#2755 = CARTESIAN_POINT ( 'NONE',  ( 8.859712399101631775, -1.914114158827161294, 13.99999999999999645 ) ) ;
#2756 = CARTESIAN_POINT ( 'NONE',  ( 7.992346231215207375, -0.9198489573344114101, 13.99999999999999645 ) ) ;
#2757 = CARTESIAN_POINT ( 'NONE',  ( -8.072272399572318236, -5.790267008923112080, 1.999999999999998224 ) ) ;
#2758 = ORIENTED_EDGE ( 'NONE', *, *, #748, .T. ) ;
#2759 = CARTESIAN_POINT ( 'NONE',  ( 8.952336951391263398, 1.032601321559316832, 1.999999999999998224 ) ) ;
#2760 =( NAMED_UNIT ( * ) PLANE_ANGLE_UNIT ( ) SI_UNIT ( $, .RADIAN. ) );
#2761 = LINE ( 'NONE', #2815, #5000 ) ;
#2762 = SHAPE_REPRESENTATION_RELATIONSHIP ( 'NONE' , 'NONE' ,  #953, #1651 ) ;
#2763 = CARTESIAN_POINT ( 'NONE',  ( 5.195030181282357162, -4.117271336869386289, 1.999999999999998224 ) ) ;
#2764 = ORIENTED_EDGE ( 'NONE', *, *, #105, .T. ) ;
#2765 = CARTESIAN_POINT ( 'NONE',  ( -6.876639332705558161, 1.598006320995754237, 1.999999999999998224 ) ) ;
#2766 = DIRECTION ( 'NONE',  ( -0.000000000000000000, -0.000000000000000000, 1.000000000000000000 ) ) ;
#2767 = LINE ( 'NONE', #230, #5124 ) ;
#2768 = APPLICATION_CONTEXT ( 'automotive_design' ) ;
#2769 = CYLINDRICAL_SURFACE ( 'NONE', #322, 22.00000000000000000 ) ;
#2770 = ORIENTED_EDGE ( 'NONE', *, *, #3650, .F. ) ;
#2771 = FACE_BOUND ( 'NONE', #2110, .T. ) ;
#2772 = CARTESIAN_POINT ( 'NONE',  ( 7.379526280503350577, 5.862399640741291940, 14.00000000000000000 ) ) ;
#2773 = CARTESIAN_POINT ( 'NONE',  ( -6.792624376349762905, -3.077375260546124203, 1.999999999999998224 ) ) ;
#2774 = CARTESIAN_POINT ( 'NONE',  ( -4.424777426321968576, -7.679192617323552739, 1.999999999999998224 ) ) ;
#2775 = CARTESIAN_POINT ( 'NONE',  ( -9.926332099419621358, -1.311590842189569894, 14.00000000000000000 ) ) ;
#2776 = ORIENTED_EDGE ( 'NONE', *, *, #4513, .F. ) ;
#2777 = CARTESIAN_POINT ( 'NONE',  ( -1.592064345877699072, 9.625584969238365929, 1.999999999999998224 ) ) ;
#2778 = CARTESIAN_POINT ( 'NONE',  ( -3.922355934210178585, -4.464780306277046584, 14.00000000000000000 ) ) ;
#2779 = CARTESIAN_POINT ( 'NONE',  ( -6.848710654519975627, 5.255840572796830479, 13.99999999999999645 ) ) ;
#2780 =( GEOMETRIC_REPRESENTATION_CONTEXT ( 3 ) GLOBAL_UNCERTAINTY_ASSIGNED_CONTEXT ( ( #3898 ) ) GLOBAL_UNIT_ASSIGNED_CONTEXT ( ( #1554, #3653, #2294 ) ) REPRESENTATION_CONTEXT ( 'NONE', 'WORKASPACE' ) );
#2781 = CARTESIAN_POINT ( 'NONE',  ( 0.2014543481397604030, 6.272771216426900942, 14.00000000000000000 ) ) ;
#2782 = ORIENTED_EDGE ( 'NONE', *, *, #1608, .F. ) ;
#2783 = CARTESIAN_POINT ( 'NONE',  ( -4.227552200850895225, 7.601683304540809871, 1.999999999999998224 ) ) ;
#2784 = CARTESIAN_POINT ( 'NONE',  ( -4.500000000000000888, 5.510910596163089556E-16, 0.000000000000000000 ) ) ;
#2785 = CARTESIAN_POINT ( 'NONE',  ( 0.2014543481397604585, 6.272771216426899166, 1.999999999999998224 ) ) ;
#2786 = ORIENTED_EDGE ( 'NONE', *, *, #1001, .F. ) ;
#2787 = CARTESIAN_POINT ( 'NONE',  ( -7.019001384594680815, 0.4577903460188660345, 1.999999999999998224 ) ) ;
#2788 = AXIS2_PLACEMENT_3D ( 'NONE', #4582, #4609, #3231 ) ;
#2789 = DIRECTION ( 'NONE',  ( 0.000000000000000000, 0.000000000000000000, -1.000000000000000000 ) ) ;
#2790 = ADVANCED_FACE ( 'NONE', ( #3344 ), #4746, .T. ) ;
#2791 = PLANE ( 'NONE',  #1172 ) ;
#2792 = AXIS2_PLACEMENT_3D ( 'NONE', #4862, #1299, #1730 ) ;
#2793 = ADVANCED_FACE ( 'NONE', ( #1043 ), #2399, .T. ) ;
#2794 = CARTESIAN_POINT ( 'NONE',  ( 2.400000000000000799, 2.449293598294705428E-16, -1.999999999999999112 ) ) ;
#2795 = VECTOR ( 'NONE', #41, 1000.000000000000000 ) ;
#2796 = SURFACE_SIDE_STYLE ('',( #1446 ) ) ;
#2797 = CARTESIAN_POINT ( 'NONE',  ( 0.000000000000000000, 0.000000000000000000, -3.300000000000000266 ) ) ;
#2798 = ORIENTED_EDGE ( 'NONE', *, *, #975, .F. ) ;
#2799 = DIRECTION ( 'NONE',  ( -1.000000000000000000, 3.540989467475305966E-16, 0.000000000000000000 ) ) ;
#2800 = CARTESIAN_POINT ( 'NONE',  ( -8.929154442179243034, -4.413097966322579779, 14.00000000000000000 ) ) ;
#2801 = CARTESIAN_POINT ( 'NONE',  ( 5.381714297850622053, -6.137309488907494170, 1.999999999999998224 ) ) ;
#2802 = CARTESIAN_POINT ( 'NONE',  ( -4.895455514773497718, -6.178604150901914061, 1.999999999999998224 ) ) ;
#2803 = CARTESIAN_POINT ( 'NONE',  ( -1.271096247112511346, -9.720655361064800104, 14.00000000000000000 ) ) ;
#2804 = EDGE_CURVE ( 'NONE', #2920, #2168, #4984, .T. ) ;
#2805 = CIRCLE ( 'NONE', #5003, 25.00000000000000000 ) ;
#2806 = CARTESIAN_POINT ( 'NONE',  ( 17.55913978494622896, -14.85518798308249266, 4.000000000000000000 ) ) ;
#2807 = VERTEX_POINT ( 'NONE', #5449 ) ;
#2808 = CARTESIAN_POINT ( 'NONE',  ( 1.380000000000002558, 21.95856267278071527, 4.000000000000000000 ) ) ;
#2809 = CARTESIAN_POINT ( 'NONE',  ( 4.443413384189735638, 4.597174039215665253, 14.00000000000000000 ) ) ;
#2810 = CARTESIAN_POINT ( 'NONE',  ( 1.176163838800443395, -10.19826953922044765, 13.99999999999999645 ) ) ;
#2811 = CARTESIAN_POINT ( 'NONE',  ( -5.021280548128706833, 3.603657539914777885, 14.00000000000094147 ) ) ;
#2812 = ORIENTED_EDGE ( 'NONE', *, *, #1842, .F. ) ;
#2813 = VECTOR ( 'NONE', #3975, 1000.000000000000000 ) ;
#2814 = CARTESIAN_POINT ( 'NONE',  ( -5.741039858921414663, -6.128965587877393872, 1.999999999999998224 ) ) ;
#2815 = CARTESIAN_POINT ( 'NONE',  ( 18.00000000000000000, 1.553654299240552096E-15, 4.000000000000000000 ) ) ;
#2816 = PRODUCT_RELATED_PRODUCT_CATEGORY ( 'part', '', ( #1195 ) ) ;
#2817 = AXIS2_PLACEMENT_3D ( 'NONE', #3801, #5219, #3861 ) ;
#2818 = SHAPE_REPRESENTATION_RELATIONSHIP ( 'NONE' , 'NONE' ,  #1911, #5006 ) ;
#2819 = CARTESIAN_POINT ( 'NONE',  ( 6.445330636073144603, -1.168293168414208827, 1.999999999999998224 ) ) ;
#2820 = ORIENTED_EDGE ( 'NONE', *, *, #3291, .T. ) ;
#2821 = CARTESIAN_POINT ( 'NONE',  ( 5.499810765991186123, -5.314180015047517358, 1.999999999999998224 ) ) ;
#2822 = DIRECTION ( 'NONE',  ( -0.000000000000000000, -0.000000000000000000, 1.000000000000000000 ) ) ;
#2823 = VECTOR ( 'NONE', #1045, 1000.000000000000000 ) ;
#2824 = CARTESIAN_POINT ( 'NONE',  ( 4.243312049792015372, -4.537448458213933833, 13.99999999999999645 ) ) ;
#2825 = CARTESIAN_POINT ( 'NONE',  ( -13.00000000000000178, 1.592040838891559293E-15, 4.000000000000003553 ) ) ;
#2826 = AXIS2_PLACEMENT_3D ( 'NONE', #1665, #5150, #4287 ) ;
#2827 = FACE_OUTER_BOUND ( 'NONE', #3761, .T. ) ;
#2828 = LINE ( 'NONE', #3342, #794 ) ;
#2829 = ORIENTED_EDGE ( 'NONE', *, *, #4629, .F. ) ;
#2830 = DIRECTION ( 'NONE',  ( -0.000000000000000000, 0.4999999999999998890, -0.8660254037844387076 ) ) ;
#2831 = CARTESIAN_POINT ( 'NONE',  ( 5.000000000000000000, 6.123233995736766282E-16, 8.000000000000000000 ) ) ;
#2832 = ADVANCED_FACE ( 'NONE', ( #1503, #5481 ), #3267, .F. ) ;
#2833 = CARTESIAN_POINT ( 'NONE',  ( 8.859712399100347469, -1.914114158827000312, 1.999999999999998224 ) ) ;
#2834 = VECTOR ( 'NONE', #4047, 1000.000000000000000 ) ;
#2835 = CARTESIAN_POINT ( 'NONE',  ( 3.713512749562912774, 8.576920285552665391, 1.999999999999998224 ) ) ;
#2836 = CARTESIAN_POINT ( 'NONE',  ( -4.424777426322135554, -7.679192617324877901, 14.00000000000000000 ) ) ;
#2837 = CARTESIAN_POINT ( 'NONE',  ( 22.00000000000000000, 0.000000000000000000, 12.00000000000000000 ) ) ;
#2838 = EDGE_LOOP ( 'NONE', ( #811, #2764, #1891, #5334 ) ) ;
#2839 = CARTESIAN_POINT ( 'NONE',  ( 10.06493078320224832, 4.366638945733749111, 1.999999999999998224 ) ) ;
#2840 = CARTESIAN_POINT ( 'NONE',  ( -6.048456868091351524, 0.8014113234714785872, 14.00000000000000000 ) ) ;
#2841 = CARTESIAN_POINT ( 'NONE',  ( 4.074896204546096357, -8.256886768010264888, 13.99999999999999645 ) ) ;
#2842 = EDGE_CURVE ( 'NONE', #5339, #4044, #3364, .T. ) ;
#2843 = CARTESIAN_POINT ( 'NONE',  ( -8.765969750979122566, 5.050798838973363125, 1.999999999999998224 ) ) ;
#2844 = VERTEX_POINT ( 'NONE', #2837 ) ;
#2845 = CARTESIAN_POINT ( 'NONE',  ( -6.848710654519973851, 5.255840572796829591, 1.999999999999998224 ) ) ;
#2846 = PRODUCT ( 'tape', 'tape', '', ( #391 ) ) ;
#2847 = DIRECTION ( 'NONE',  ( -1.000000000000000000, 0.000000000000000000, -0.000000000000000000 ) ) ;
#2848 = CARTESIAN_POINT ( 'NONE',  ( -3.987231204391976203, 4.693390172671164429, 1.999999999999412914 ) ) ;
#2849 = ORIENTED_EDGE ( 'NONE', *, *, #1636, .T. ) ;
#2850 = CARTESIAN_POINT ( 'NONE',  ( 3.247347166530788698, 6.590896817052186663, 1.999999999999998224 ) ) ;
#2851 = FACE_BOUND ( 'NONE', #851, .T. ) ;
#2852 = CARTESIAN_POINT ( 'NONE',  ( -0.4015567206216588692, -6.330257989742014146, 13.99999999999999645 ) ) ;
#2853 = CYLINDRICAL_SURFACE ( 'NONE', #414, 22.50000000000000355 ) ;
#2854 = CARTESIAN_POINT ( 'NONE',  ( 0.000000000000000000, 0.000000000000000000, 15.94994774640597512 ) ) ;
#2855 = VERTEX_POINT ( 'NONE', #1542 ) ;
#2856 = DIRECTION ( 'NONE',  ( -0.000000000000000000, -0.000000000000000000, 1.000000000000000000 ) ) ;
#2857 = CARTESIAN_POINT ( 'NONE',  ( 9.602236826902712963, 4.172718697305597857, 14.00000000000000000 ) ) ;
#2858 = CARTESIAN_POINT ( 'NONE',  ( 6.971023843911450690, -5.915260676233723203, 1.999999999999998224 ) ) ;
#2859 = CARTESIAN_POINT ( 'NONE',  ( -1.484422800923361985, -8.172499773498691056, 13.99999999999999645 ) ) ;
#2860 = CARTESIAN_POINT ( 'NONE',  ( 4.264126983937992499, 9.433107915010287670, 14.00000000000000000 ) ) ;
#2861 = VERTEX_POINT ( 'NONE', #4131 ) ;
#2862 = PLANE ( 'NONE',  #5201 ) ;
#2863 = ORIENTED_EDGE ( 'NONE', *, *, #1175, .T. ) ;
#2864 = CARTESIAN_POINT ( 'NONE',  ( 17.99999999999999289, -17.34935157289748631, 8.000000000000000000 ) ) ;
#2865 = CARTESIAN_POINT ( 'NONE',  ( 7.494325059173605474, -0.8592991332473474131, 14.00000000000000000 ) ) ;
#2866 = ADVANCED_FACE ( 'NONE', ( #185 ), #2862, .F. ) ;
#2867 = CARTESIAN_POINT ( 'NONE',  ( -4.679820741050984445, -8.111215689329295486, 13.99999999999999645 ) ) ;
#2868 = CARTESIAN_POINT ( 'NONE',  ( -1.105557477332586691, -6.708264047591377732, 14.00000000000000000 ) ) ;
#2869 = VERTEX_POINT ( 'NONE', #5047 ) ;
#2870 = CARTESIAN_POINT ( 'NONE',  ( -10.26372689808571970, -2.219791875069699216, 1.999999999999998224 ) ) ;
#2871 =( GEOMETRIC_REPRESENTATION_CONTEXT ( 3 ) GLOBAL_UNCERTAINTY_ASSIGNED_CONTEXT ( ( #5500 ) ) GLOBAL_UNIT_ASSIGNED_CONTEXT ( ( #5407, #4569, #3701 ) ) REPRESENTATION_CONTEXT ( 'NONE', 'WORKASPACE' ) );
#2872 = CARTESIAN_POINT ( 'NONE',  ( 0.000000000000000000, 0.000000000000000000, 12.00000000000000000 ) ) ;
#2873 = CARTESIAN_POINT ( 'NONE',  ( 3.622712361020122618, 5.236663886535374957, 1.999999999999998224 ) ) ;
#2874 = VERTEX_POINT ( 'NONE', #240 ) ;
#2875 = CARTESIAN_POINT ( 'NONE',  ( 0.5542950790998156796, -6.736796398737814329, 1.999999999999998224 ) ) ;
#2876 = CARTESIAN_POINT ( 'NONE',  ( -4.256527737015712631, -4.845957569453684499, 1.999999999999998224 ) ) ;
#2877 = DIRECTION ( 'NONE',  ( 0.06000000000000009492, 0.9981983770774225384, 0.000000000000000000 ) ) ;
#2878 = CARTESIAN_POINT ( 'NONE',  ( 23.00000000000000000, -2.168404344971008868E-16, -16.41957833606399930 ) ) ;
#2879 = DIRECTION ( 'NONE',  ( 0.000000000000000000, 1.224646799147353207E-16, -1.000000000000000000 ) ) ;
#2880 = VERTEX_POINT ( 'NONE', #2806 ) ;
#2881 = CARTESIAN_POINT ( 'NONE',  ( 1.300000000000000044, -0.7216878364870318308, -1.250000000000000000 ) ) ;
#2882 = DIRECTION ( 'NONE',  ( -1.000000000000000000, 0.000000000000000000, 0.000000000000000000 ) ) ;
#2883 = CARTESIAN_POINT ( 'NONE',  ( -3.290073422422500560, -8.739709727800574868, 1.999999999999998224 ) ) ;
#2884 = CIRCLE ( 'NONE', #4353, 5.000000000000000000 ) ;
#2885 = CARTESIAN_POINT ( 'NONE',  ( 5.103689747953259470, 6.014827819656690444, 13.99999999999999645 ) ) ;
#2886 = CARTESIAN_POINT ( 'NONE',  ( 5.000000000000001776, 24.49489742783178414, 24.08672805191341482 ) ) ;
#2887 = ORIENTED_EDGE ( 'NONE', *, *, #3014, .F. ) ;
#2888 = PRODUCT_DEFINITION_SHAPE ( 'NONE', 'NONE',  #5690 ) ;
#2889 = DIRECTION ( 'NONE',  ( 1.000000000000000000, 0.000000000000000000, 0.000000000000000000 ) ) ;
#2890 = EDGE_LOOP ( 'NONE', ( #3511, #751, #2633, #1769 ) ) ;
#2891 = CARTESIAN_POINT ( 'NONE',  ( 8.671201137383034663, 6.657490096169006222, 1.999999999999998224 ) ) ;
#2892 = AXIS2_PLACEMENT_3D ( 'NONE', #4521, #926, #146 ) ;
#2893 = CARTESIAN_POINT ( 'NONE',  ( 0.9466184546083361573, 7.233353930637703044, 14.00000000000000000 ) ) ;
#2894 = CARTESIAN_POINT ( 'NONE',  ( 6.971023843911450690, -5.915260676233724091, 13.99999999999999645 ) ) ;
#2895 = VECTOR ( 'NONE', #1003, 1000.000000000000000 ) ;
#2896 = EDGE_CURVE ( 'NONE', #247, #3586, #1479, .T. ) ;
#2897 = CARTESIAN_POINT ( 'NONE',  ( 6.340368144647111848, -1.697206311171021831, 14.00000000000000000 ) ) ;
#2898 = EDGE_LOOP ( 'NONE', ( #1106, #2043, #204, #789 ) ) ;
#2899 = CARTESIAN_POINT ( 'NONE',  ( 3.917689075872947235, 9.035181080458078995, 1.999999999999998224 ) ) ;
#2900 = AXIS2_PLACEMENT_3D ( 'NONE', #1533, #3713, #5132 ) ;
#2901 = CYLINDRICAL_SURFACE ( 'NONE', #3904, 15.00000000000000000 ) ;
#2902 = DIRECTION ( 'NONE',  ( 1.000000000000000000, 0.000000000000000000, 0.000000000000000000 ) ) ;
#2903 = CARTESIAN_POINT ( 'NONE',  ( -3.391372024942433505, 7.476497417048837413, 1.999999999999998224 ) ) ;
#2904 = AXIS2_PLACEMENT_3D ( 'NONE', #4644, #3353, #733 ) ;
#2905 = CARTESIAN_POINT ( 'NONE',  ( 0.5141566911143078400, -7.748312628312726602, 1.999999999999998224 ) ) ;
#2906 = CARTESIAN_POINT ( 'NONE',  ( 0.7762864403411611214, 6.746413643992394960, 1.999999999999998224 ) ) ;
#2907 = CARTESIAN_POINT ( 'NONE',  ( -0.2539011084976132149, 7.766605221862832309, 13.99999999999999645 ) ) ;
#2908 = EDGE_CURVE ( 'NONE', #660, #2869, #1105, .T. ) ;
#2909 = DIRECTION ( 'NONE',  ( 0.9999273757268464236, -0.01205169166640781934, 0.000000000000000000 ) ) ;
#2910 =( NAMED_UNIT ( * ) SI_UNIT ( $, .STERADIAN. ) SOLID_ANGLE_UNIT ( ) );
#2911 = ORIENTED_EDGE ( 'NONE', *, *, #2228, .F. ) ;
#2912 = DIRECTION ( 'NONE',  ( -0.000000000000000000, -0.000000000000000000, 1.000000000000000000 ) ) ;
#2913 = DIRECTION ( 'NONE',  ( 0.000000000000000000, 0.000000000000000000, -1.000000000000000000 ) ) ;
#2914 = CARTESIAN_POINT ( 'NONE',  ( -3.594774944545354511, 7.935102286573618713, 1.999999999999998224 ) ) ;
#2915 = AXIS2_PLACEMENT_3D ( 'NONE', #3917, #1754, #5671 ) ;
#2916 = CARTESIAN_POINT ( 'NONE',  ( -7.080399483669658878, -6.208478756603783566, 13.99999999999999645 ) ) ;
#2917 = LINE ( 'NONE', #1163, #4262 ) ;
#2918 = ORIENTED_EDGE ( 'NONE', *, *, #3966, .T. ) ;
#2919 = LINE ( 'NONE', #2051, #3181 ) ;
#2920 = VERTEX_POINT ( 'NONE', #2001 ) ;
#2921 = CONICAL_SURFACE ( 'NONE', #4119, 2.000000000000000000, 1.029744258676656532 ) ;
#2922 = PLANE ( 'NONE',  #1903 ) ;
#2923 = CARTESIAN_POINT ( 'NONE',  ( -6.881333183081246752, -1.254343363641206688, 14.00000000000000000 ) ) ;
#2924 = CARTESIAN_POINT ( 'NONE',  ( 7.233280636258937690, 6.778630567624380099, 13.99999999999999645 ) ) ;
#2925 = CARTESIAN_POINT ( 'NONE',  ( -4.975175822334874098, 5.137265612443751017, 14.00000000000000000 ) ) ;
#2926 = ORIENTED_EDGE ( 'NONE', *, *, #4980, .F. ) ;
#2927 = CARTESIAN_POINT ( 'NONE',  ( 9.077580196902394150, 4.112174628513753483, 1.999999999999998224 ) ) ;
#2928 = EDGE_CURVE ( 'NONE', #30, #3011, #2441, .T. ) ;
#2929 = CARTESIAN_POINT ( 'NONE',  ( 4.999999999999923617, 22.44994432064366308, -8.000000000000000000 ) ) ;
#2930 = DIRECTION ( 'NONE',  ( 1.000000000000000000, 0.000000000000000000, 0.000000000000000000 ) ) ;
#2931 = CARTESIAN_POINT ( 'NONE',  ( 7.494325059173603698, -0.8592991332473469690, 1.999999999999998224 ) ) ;
#2932 = DIRECTION ( 'NONE',  ( 0.000000000000000000, 0.000000000000000000, 1.000000000000000000 ) ) ;
#2933 = CARTESIAN_POINT ( 'NONE',  ( 6.180183843827204093, 3.174252413088802793, 13.99999999999999645 ) ) ;
#2934 =( NAMED_UNIT ( * ) PLANE_ANGLE_UNIT ( ) SI_UNIT ( $, .RADIAN. ) );
#2935 = CARTESIAN_POINT ( 'NONE',  ( -3.609299841826103972, -9.156952235374472338, 1.999999999999998224 ) ) ;
#2936 = CARTESIAN_POINT ( 'NONE',  ( 2.149999999999999467, 0.000000000000000000, -3.100000000000000533 ) ) ;
#2937 = CARTESIAN_POINT ( 'NONE',  ( 1.300000000000000044, 0.7216878364870328300, 1.249999999999999778 ) ) ;
#2938 = EDGE_LOOP ( 'NONE', ( #4203, #3297, #3304, #934 ) ) ;
#2939 = CARTESIAN_POINT ( 'NONE',  ( 5.000000000000000000, -6.123233995736766282E-16, -2.000000000000000000 ) ) ;
#2940 = PLANE ( 'NONE',  #2164 ) ;
#2941 = CARTESIAN_POINT ( 'NONE',  ( -9.247353065533557626, -2.155497948345702408, 1.999999999999998224 ) ) ;
#2942 = CARTESIAN_POINT ( 'NONE',  ( -2.557952627993306471, -8.967547948949398773, 13.99999999999999645 ) ) ;
#2943 = CARTESIAN_POINT ( 'NONE',  ( 0.000000000000000000, 0.000000000000000000, -4.000000000000000000 ) ) ;
#2944 = ORIENTED_EDGE ( 'NONE', *, *, #5079, .T. ) ;
#2945 = CYLINDRICAL_SURFACE ( 'NONE', #1707, 4.500000000000000888 ) ;
#2946 = VERTEX_POINT ( 'NONE', #4590 ) ;
#2947 = CARTESIAN_POINT ( 'NONE',  ( 1.380000000000002336, 22.95856267278071172, 15.94994774640597512 ) ) ;
#2948 = CARTESIAN_POINT ( 'NONE',  ( 2.690160903457257557, 6.823041841979409661, 14.00000000000000000 ) ) ;
#2949 = CARTESIAN_POINT ( 'NONE',  ( 6.769338797470518365, 8.534199679355843671, 13.99999999999999645 ) ) ;
#2950 = EDGE_CURVE ( 'NONE', #4444, #4755, #2460, .T. ) ;
#2951 = CARTESIAN_POINT ( 'NONE',  ( 7.494325059173605474, -0.8592991332473474131, 14.00000000000000000 ) ) ;
#2952 = APPLICATION_CONTEXT ( 'automotive_design' ) ;
#2953 = VERTEX_POINT ( 'NONE', #3722 ) ;
#2954 = CARTESIAN_POINT ( 'NONE',  ( 0.3355163285737912116, -10.27362971114624024, 1.999999999999998224 ) ) ;
#2955 = AXIS2_PLACEMENT_3D ( 'NONE', #4976, #1932, #5504 ) ;
#2956 = EDGE_CURVE ( 'NONE', #4096, #4488, #674, .T. ) ;
#2957 = CARTESIAN_POINT ( 'NONE',  ( -22.50000000000000355, 0.000000000000000000, 4.000000000000000000 ) ) ;
#2958 = DIRECTION ( 'NONE',  ( 0.000000000000000000, 0.000000000000000000, 1.000000000000000000 ) ) ;
#2959 = CARTESIAN_POINT ( 'NONE',  ( -7.425829140954076202, 3.215541426300492223, 1.999999999999998224 ) ) ;
#2960 = DIRECTION ( 'NONE',  ( 1.000000000000000000, 0.000000000000000000, 0.000000000000000000 ) ) ;
#2961 = CARTESIAN_POINT ( 'NONE',  ( -0.5931392160223127874, -7.263020831007573896, 13.99999999999999645 ) ) ;
#2962 =( GEOMETRIC_REPRESENTATION_CONTEXT ( 3 ) GLOBAL_UNCERTAINTY_ASSIGNED_CONTEXT ( ( #575 ) ) GLOBAL_UNIT_ASSIGNED_CONTEXT ( ( #4830, #4454, #83 ) ) REPRESENTATION_CONTEXT ( 'NONE', 'WORKASPACE' ) );
#2963 = SURFACE_SIDE_STYLE ('',( #5152 ) ) ;
#2964 = CARTESIAN_POINT ( 'NONE',  ( 6.721134410589269415, -6.938257756003234356, 1.999999999999998224 ) ) ;
#2965 = EDGE_CURVE ( 'NONE', #5441, #2844, #3091, .T. ) ;
#2966 = CARTESIAN_POINT ( 'NONE',  ( 0.000000000000000000, 0.000000000000000000, 4.000000000000000000 ) ) ;
#2967 = LINE ( 'NONE', #4715, #5472 ) ;
#2968 = ORIENTED_EDGE ( 'NONE', *, *, #1177, .T. ) ;
#2969 = CARTESIAN_POINT ( 'NONE',  ( 5.000000000000001776, 24.49489742783178414, 12.00000000000000000 ) ) ;
#2970 = ITEM_DEFINED_TRANSFORMATION ( 'NONE', 'NONE', #4255,  #1336 ) ;
#2971 = DIRECTION ( 'NONE',  ( 0.000000000000000000, 0.000000000000000000, -1.000000000000000000 ) ) ;
#2972 = CARTESIAN_POINT ( 'NONE',  ( 7.748217264258252968, 4.472783157626409434, 13.99999999999999645 ) ) ;
#2973 = CARTESIAN_POINT ( 'NONE',  ( -8.765969750978372943, 5.050798838973364902, 14.00000000000000000 ) ) ;
#2974 = ORIENTED_EDGE ( 'NONE', *, *, #752, .F. ) ;
#2975 = PLANE ( 'NONE',  #2628 ) ;
#2976 = ORIENTED_EDGE ( 'NONE', *, *, #224, .F. ) ;
#2977 = CARTESIAN_POINT ( 'NONE',  ( 4.500000000000000000, 0.000000000000000000, -3.100000000000000533 ) ) ;
#2978 = CARTESIAN_POINT ( 'NONE',  ( 3.810368753942760200, 7.433568398487740758, 14.00000000000000000 ) ) ;
#2979 = CARTESIAN_POINT ( 'NONE',  ( -3.886954398759499885, 5.424498719065524277, 1.999999999999998224 ) ) ;
#2980 = AXIS2_PLACEMENT_3D ( 'NONE', #2943, #238, #4695 ) ;
#2981 = EDGE_CURVE ( 'NONE', #4872, #3918, #4218, .T. ) ;
#2982 = CARTESIAN_POINT ( 'NONE',  ( 5.000000000000000000, 6.123233995736766282E-16, 2.000000000000000000 ) ) ;
#2983 = CARTESIAN_POINT ( 'NONE',  ( 4.776808680784973227, 5.634249062854204126, 14.00000000000000000 ) ) ;
#2984 = AXIS2_PLACEMENT_3D ( 'NONE', #3448, #430, #5241 ) ;
#2985 = ORIENTED_EDGE ( 'NONE', *, *, #3745, .T. ) ;
#2986 = CARTESIAN_POINT ( 'NONE',  ( -9.381622446299669349, -4.629808687489259889, 1.999999999999998224 ) ) ;
#2987 = PRODUCT_DEFINITION_SHAPE ( 'NONE', 'NONE',  #177 ) ;
#2988 = CARTESIAN_POINT ( 'NONE',  ( 5.000000000000000000, 6.123233995736766282E-16, 8.000000000000000000 ) ) ;
#2989 =( LENGTH_UNIT ( ) NAMED_UNIT ( * ) SI_UNIT ( .MILLI., .METRE. ) );
#2990 =( REPRESENTATION_RELATIONSHIP ('NONE','NONE', #4854, #143 ) REPRESENTATION_RELATIONSHIP_WITH_TRANSFORMATION ( #2970 )SHAPE_REPRESENTATION_RELATIONSHIP( ) );
#2991 = CARTESIAN_POINT ( 'NONE',  ( 8.453438707198472457, 0.9797652757261496870, 1.999999999999998224 ) ) ;
#2992 = AXIS2_PLACEMENT_3D ( 'NONE', #4583, #2393, #207 ) ;
#2993 = LINE ( 'NONE', #2096, #4298 ) ;
#2994 = CARTESIAN_POINT ( 'NONE',  ( -1.424809953814591523, 6.586142414399822620, 13.99999999999999645 ) ) ;
#2995 = ADVANCED_FACE ( 'NONE', ( #3325, #1165 ), #3782, .T. ) ;
#2996 = AXIS2_PLACEMENT_3D ( 'NONE', #2562, #1699, #3453 ) ;
#2997 = DIRECTION ( 'NONE',  ( 0.000000000000000000, 0.000000000000000000, 1.000000000000000000 ) ) ;
#2998 = CARTESIAN_POINT ( 'NONE',  ( -0.7616497023963333390, 9.236585841460744462, 1.999999999999998224 ) ) ;
#2999 = CARTESIAN_POINT ( 'NONE',  ( 4.999999999999923617, 22.44994432064366308, -8.000000000000000000 ) ) ;
#3000 = DIRECTION ( 'NONE',  ( 0.000000000000000000, 0.000000000000000000, 1.000000000000000000 ) ) ;
#3001 = ORIENTED_EDGE ( 'NONE', *, *, #257, .T. ) ;
#3002 = TOROIDAL_SURFACE ( 'NONE', #2636, 2.199999999999999289, 0.2000000000000000111 ) ;
#3003 = FACE_OUTER_BOUND ( 'NONE', #3402, .T. ) ;
#3004 = PLANE ( 'NONE',  #4729 ) ;
#3005 = CARTESIAN_POINT ( 'NONE',  ( -8.745075223331019387, 3.959260399367729111, 13.99999999999999645 ) ) ;
#3006 = VECTOR ( 'NONE', #4151, 1000.000000000000000 ) ;
#3007 = LINE ( 'NONE', #463, #1870 ) ;
#3008 = ORIENTED_EDGE ( 'NONE', *, *, #3504, .T. ) ;
#3009 = CARTESIAN_POINT ( 'NONE',  ( 10.50003631213657940, 0.006025845833179013789, 7.999999999999998224 ) ) ;
#3010 = EDGE_CURVE ( 'NONE', #11, #1449, #2919, .T. ) ;
#3011 = VERTEX_POINT ( 'NONE', #4242 ) ;
#3012 = DIRECTION ( 'NONE',  ( 0.000000000000000000, -1.000000000000000000, 0.000000000000000000 ) ) ;
#3013 = CARTESIAN_POINT ( 'NONE',  ( -7.301858691287087311, -3.172613069824385956, 14.00000000000000000 ) ) ;
#3014 = EDGE_CURVE ( 'NONE', #3426, #4851, #293, .T. ) ;
#3015 = CARTESIAN_POINT ( 'NONE',  ( -1.451466707715830973, -6.203196315423896934, 1.999999999999998224 ) ) ;
#3016 = VECTOR ( 'NONE', #3387, 1000.000000000000000 ) ;
#3017 = DIRECTION ( 'NONE',  ( 0.000000000000000000, 0.000000000000000000, 1.000000000000000000 ) ) ;
#3018 = CARTESIAN_POINT ( 'NONE',  ( 5.499810765991187012, -5.314180015047230476, 14.00000000000000000 ) ) ;
#3019 = EDGE_LOOP ( 'NONE', ( #1104, #4323, #609, #5026, #2026 ) ) ;
#3020 = CARTESIAN_POINT ( 'NONE',  ( -3.287100391418392942, 10.22059872437900019, 1.999999999999998224 ) ) ;
#3021 = CONICAL_SURFACE ( 'NONE', #5314, 1732.050807568856271, 1.047197551196592524 ) ;
#3022 = EDGE_CURVE ( 'NONE', #1000, #1950, #5225, .T. ) ;
#3023 = CARTESIAN_POINT ( 'NONE',  ( -6.551010013419181988, 0.8677952034721571062, 13.99999999999999645 ) ) ;
#3024 = PRODUCT_CONTEXT ( 'NONE', #2071, 'mechanical' ) ;
#3025 = CARTESIAN_POINT ( 'NONE',  ( -8.013356705133178437, 0.6503825268544296545, 1.999999999999998224 ) ) ;
#3026 = CARTESIAN_POINT ( 'NONE',  ( 6.209839678910233474, -3.451293940533043614, 1.999999999999998224 ) ) ;
#3027 = CARTESIAN_POINT ( 'NONE',  ( -7.519441789400338472, 0.4931591957933217363, 13.99999999999999645 ) ) ;
#3028 = DIRECTION ( 'NONE',  ( 1.000000000000000000, 4.364351673553916694E-15, 0.000000000000000000 ) ) ;
#3029 = CARTESIAN_POINT ( 'NONE',  ( -6.681386044268610824, 6.252046474378027519, 1.999999999999998224 ) ) ;
#3030 = CARTESIAN_POINT ( 'NONE',  ( 0.000000000000000000, 0.7216878364870328300, -1.250000000000000000 ) ) ;
#3031 = PRESENTATION_STYLE_ASSIGNMENT (( #5586 ) ) ;
#3032 = ORIENTED_EDGE ( 'NONE', *, *, #4813, .T. ) ;
#3033 = CARTESIAN_POINT ( 'NONE',  ( 0.000000000000000000, 0.000000000000000000, 14.00000000000000000 ) ) ;
#3034 = CARTESIAN_POINT ( 'NONE',  ( 5.347643153870340171, -7.463670412150953837, 13.99999999999999645 ) ) ;
#3035 = CARTESIAN_POINT ( 'NONE',  ( 0.000000000000000000, 0.7216878364870328300, 1.249999999999999778 ) ) ;
#3036 = ORIENTED_EDGE ( 'NONE', *, *, #4681, .F. ) ;
#3037 = CARTESIAN_POINT ( 'NONE',  ( 5.000000000000001776, 24.49489742783178414, 24.08672805191341482 ) ) ;
#3038 = ORIENTED_EDGE ( 'NONE', *, *, #3592, .F. ) ;
#3039 = DIRECTION ( 'NONE',  ( 0.000000000000000000, 0.000000000000000000, -1.000000000000000000 ) ) ;
#3040 = CARTESIAN_POINT ( 'NONE',  ( -1.001529162299639619, -8.740421795711004194, 14.00000000000000000 ) ) ;
#3041 = CARTESIAN_POINT ( 'NONE',  ( -8.741731599017841248, 6.051300285686072478, 13.99999999999999645 ) ) ;
#3042 = UNCERTAINTY_MEASURE_WITH_UNIT (LENGTH_MEASURE( 1.000000000000000082E-05 ), #3419, 'distance_accuracy_value', 'NONE');
#3043 = CARTESIAN_POINT ( 'NONE',  ( -5.000000000000000000, 4.999999999999978684, 5.000000000000000000 ) ) ;
#3044 = CARTESIAN_POINT ( 'NONE',  ( -3.813875884798381577, -6.869235835554827752, 14.00000000000000000 ) ) ;
#3045 = EDGE_CURVE ( 'NONE', #2508, #5647, #4723, .T. ) ;
#3046 = VERTEX_POINT ( 'NONE', #5137 ) ;
#3047 = CARTESIAN_POINT ( 'NONE',  ( 0.000000000000000000, 0.000000000000000000, -3.100000000000000533 ) ) ;
#3048 = ADVANCED_FACE ( 'NONE', ( #787 ), #422, .T. ) ;
#3049 = EDGE_CURVE ( 'NONE', #841, #465, #1626, .T. ) ;
#3050 = CARTESIAN_POINT ( 'NONE',  ( 3.892125705850195683, -6.036954802193643665, 13.99999999999999645 ) ) ;
#3051 = CARTESIAN_POINT ( 'NONE',  ( 1.511842404626676961, 9.183516746439465805, 1.999999999999998224 ) ) ;
#3052 = CARTESIAN_POINT ( 'NONE',  ( 2.406079317367887160, 6.392288322179701332, 1.999999999999998224 ) ) ;
#3053 = CARTESIAN_POINT ( 'NONE',  ( 4.683456943470878819, 7.530568860026274791, 13.99999999999999645 ) ) ;
#3054 = DIRECTION ( 'NONE',  ( -4.364351673553916694E-15, 1.000000000000000000, 0.000000000000000000 ) ) ;
#3055 = FILL_AREA_STYLE_COLOUR ( '', #759 ) ;
#3056 = FACE_OUTER_BOUND ( 'NONE', #1679, .T. ) ;
#3057 = ADVANCED_FACE ( 'NONE', ( #1282, #4808 ), #2509, .T. ) ;
#3058 = CARTESIAN_POINT ( 'NONE',  ( 1.380000000000002336, 22.95856267278071172, 4.000000000000000000 ) ) ;
#3059 = DIRECTION ( 'NONE',  ( -0.000000000000000000, -0.000000000000000000, 1.000000000000000000 ) ) ;
#3060 = ORIENTED_EDGE ( 'NONE', *, *, #4668, .F. ) ;
#3061 = DIRECTION ( 'NONE',  ( -0.000000000000000000, -0.000000000000000000, 1.000000000000000000 ) ) ;
#3062 = CARTESIAN_POINT ( 'NONE',  ( -2.440069559021786905, 10.46881825416662259, 13.99999999999999645 ) ) ;
#3063 = ORIENTED_EDGE ( 'NONE', *, *, #1295, .T. ) ;
#3064 = CARTESIAN_POINT ( 'NONE',  ( 0.000000000000000000, 0.000000000000000000, 14.00000000000000000 ) ) ;
#3065 = EDGE_LOOP ( 'NONE', ( #4784, #4891, #2631, #379, #3258, #4716, #2418, #872, #3280 ) ) ;
#3066 = EDGE_LOOP ( 'NONE', ( #1884, #780, #4998, #5503 ) ) ;
#3067 = CARTESIAN_POINT ( 'NONE',  ( -8.013356705133178437, 0.6503825268544297655, 14.00000000000000000 ) ) ;
#3068 = CARTESIAN_POINT ( 'NONE',  ( 2.597146444261841491, -5.700021143261159828, 1.999999999999998224 ) ) ;
#3069 =( REPRESENTATION_RELATIONSHIP ('NONE','NONE', #4854, #1362 ) REPRESENTATION_RELATIONSHIP_WITH_TRANSFORMATION ( #1293 )SHAPE_REPRESENTATION_RELATIONSHIP( ) );
#3070 = CARTESIAN_POINT ( 'NONE',  ( -1.379999999999999893, 22.95856267278071172, 11.00000000000000000 ) ) ;
#3071 = EDGE_CURVE ( 'NONE', #2880, #3426, #50, .T. ) ;
#3072 = CARTESIAN_POINT ( 'NONE',  ( -2.138212235155100061, 7.953261502403491612, 14.00000000000000000 ) ) ;
#3073 = EDGE_CURVE ( 'NONE', #2869, #3473, #4302, .T. ) ;
#3074 = EDGE_LOOP ( 'NONE', ( #4007, #165, #2052, #5138 ) ) ;
#3075 = CIRCLE ( 'NONE', #5456, 0.2500000000000002220 ) ;
#3076 = DIRECTION ( 'NONE',  ( -1.000000000000000000, 0.000000000000000000, 0.000000000000000000 ) ) ;
#3077 = CARTESIAN_POINT ( 'NONE',  ( -2.965071238690786259, 6.007415411094351398, 13.99999999999999645 ) ) ;
#3078 = AXIS2_PLACEMENT_3D ( 'NONE', #3043, #5684, #3497 ) ;
#3079 = APPLICATION_PROTOCOL_DEFINITION ( 'draft international standard', 'automotive_design', 1998, #2952 ) ;
#3080 = CARTESIAN_POINT ( 'NONE',  ( 5.612687125617794592, -6.603876269260512188, 1.999999999999998224 ) ) ;
#3081 = CARTESIAN_POINT ( 'NONE',  ( 6.824478893064961582, -1.828844244265459329, 1.999999999999998224 ) ) ;
#3082 = VECTOR ( 'NONE', #1947, 1000.000000000000000 ) ;
#3083 = PLANE ( 'NONE',  #1506 ) ;
#3084 = CARTESIAN_POINT ( 'NONE',  ( 7.108868828250527905, 7.597268273414325535, 1.999999999999998224 ) ) ;
#3085 = TOROIDAL_SURFACE ( 'NONE', #1054, 2.199999999999999289, 0.2000000000000000111 ) ;
#3086 = CARTESIAN_POINT ( 'NONE',  ( 2.389076732465379216, -5.237771676861643577, 1.999999999999998224 ) ) ;
#3087 = DIRECTION ( 'NONE',  ( 0.000000000000000000, 0.000000000000000000, 1.000000000000000000 ) ) ;
#3088 = VERTEX_POINT ( 'NONE', #1306 ) ;
#3089 = LINE ( 'NONE', #1327, #981 ) ;
#3090 = EDGE_CURVE ( 'NONE', #2746, #5009, #233, .T. ) ;
#3091 = CIRCLE ( 'NONE', #5660, 22.00000000000000000 ) ;
#3092 = CARTESIAN_POINT ( 'NONE',  ( 5.279590631142085044, 9.498297537455629325, 13.99999999999999645 ) ) ;
#3093 = EDGE_LOOP ( 'NONE', ( #2092, #3492, #2147, #986, #5188, #5271, #4188, #150 ) ) ;
#3094 = DIRECTION ( 'NONE',  ( 1.000000000000000000, 0.000000000000000000, 0.000000000000000000 ) ) ;
#3095 = ORIENTED_EDGE ( 'NONE', *, *, #5283, .T. ) ;
#3096 = LINE ( 'NONE', #3581, #710 ) ;
#3097 = CARTESIAN_POINT ( 'NONE',  ( -7.945923533235638381, 1.308497053349305883, 14.00000000000000000 ) ) ;
#3098 = CARTESIAN_POINT ( 'NONE',  ( -7.375360291558941128, -1.341686286798741135, 1.999999999999998224 ) ) ;
#3099 = AXIS2_PLACEMENT_3D ( 'NONE', #3888, #5641, #521 ) ;
#3100 = DIRECTION ( 'NONE',  ( -0.000000000000000000, -0.000000000000000000, 1.000000000000000000 ) ) ;
#3101 = CARTESIAN_POINT ( 'NONE',  ( 5.059064342543619475, -7.053288479152013402, 14.00000000000000000 ) ) ;
#3102 = EDGE_LOOP ( 'NONE', ( #1513, #2625, #2488, #2659 ) ) ;
#3103 = VECTOR ( 'NONE', #1224, 1000.000000000000000 ) ;
#3104 = CARTESIAN_POINT ( 'NONE',  ( 0.7976699882155456889, 9.763020831628287155, 1.999999999999998224 ) ) ;
#3105 = DIRECTION ( 'NONE',  ( -0.000000000000000000, -0.000000000000000000, 1.000000000000000000 ) ) ;
#3106 = CARTESIAN_POINT ( 'NONE',  ( -6.792624376349764681, -3.077375260545992752, 13.99999999999999645 ) ) ;
#3107 = AXIS2_PLACEMENT_3D ( 'NONE', #1107, #5451, #272 ) ;
#3108 = ITEM_DEFINED_TRANSFORMATION ( 'NONE', 'NONE', #4529,  #1336 ) ;
#3109 = CARTESIAN_POINT ( 'NONE',  ( 7.258279873955303607, -6.354128476750924293, 1.999999999999998224 ) ) ;
#3110 = CARTESIAN_POINT ( 'NONE',  ( -2.919577271296705412, -6.733962781534540198, 1.999999999999998224 ) ) ;
#3111 = DIRECTION ( 'NONE',  ( 0.000000000000000000, 0.000000000000000000, -1.000000000000000000 ) ) ;
#3112 = UNCERTAINTY_MEASURE_WITH_UNIT (LENGTH_MEASURE( 1.000000000000000082E-05 ), #3372, 'distance_accuracy_value', 'NONE');
#3113 = LINE ( 'NONE', #3569, #3529 ) ;
#3114 = SHAPE_REPRESENTATION_RELATIONSHIP ( 'NONE' , 'NONE' ,  #4116, #1852 ) ;
#3115 = FACE_OUTER_BOUND ( 'NONE', #4066, .T. ) ;
#3116 = CARTESIAN_POINT ( 'NONE',  ( -3.110890340275366039, -5.031137978950550149, 1.999999999999998224 ) ) ;
#3117 = CARTESIAN_POINT ( 'NONE',  ( 0.000000000000000000, 0.000000000000000000, -8.000000000000000000 ) ) ;
#3118 = EDGE_LOOP ( 'NONE', ( #471, #5038, #372, #5083 ) ) ;
#3119 = SURFACE_SIDE_STYLE ('',( #5353 ) ) ;
#3120 = CARTESIAN_POINT ( 'NONE',  ( -10.42442484909544653, -1.371544430045602558, 13.99999999999999645 ) ) ;
#3121 = DIRECTION ( 'NONE',  ( 0.000000000000000000, 0.000000000000000000, 1.000000000000000000 ) ) ;
#3122 = FACE_OUTER_BOUND ( 'NONE', #3789, .T. ) ;
#3123 = ORIENTED_EDGE ( 'NONE', *, *, #2292, .T. ) ;
#3124 = ORIENTED_EDGE ( 'NONE', *, *, #687, .T. ) ;
#3125 = CARTESIAN_POINT ( 'NONE',  ( -8.999716648909560135, -0.5976852874978595409, 14.00000000000000000 ) ) ;
#3126 = CARTESIAN_POINT ( 'NONE',  ( 7.937472058416057408, 1.044590838406009414, 1.999999999999998224 ) ) ;
#3127 = CARTESIAN_POINT ( 'NONE',  ( -7.301858691287086423, -3.172613069824385068, 1.999999999999998224 ) ) ;
#3128 = CARTESIAN_POINT ( 'NONE',  ( -3.231338468933152797, -7.147216519672495494, 14.00000000000000000 ) ) ;
#3129 = ORIENTED_EDGE ( 'NONE', *, *, #3980, .T. ) ;
#3130 = CARTESIAN_POINT ( 'NONE',  ( 8.697835924490032511, 4.836984431370230375, 1.999999999999998224 ) ) ;
#3131 = CARTESIAN_POINT ( 'NONE',  ( 5.000000000000000000, 5.000000000000022204, -5.000000000000000000 ) ) ;
#3132 = EDGE_CURVE ( 'NONE', #4301, #1496, #5189, .T. ) ;
#3133 = CARTESIAN_POINT ( 'NONE',  ( 5.806279480218260680, -1.975834710110475401, 13.99999999999999645 ) ) ;
#3134 = CONTEXT_DEPENDENT_SHAPE_REPRESENTATION ( #2691, #2888 ) ;
#3135 = CARTESIAN_POINT ( 'NONE',  ( -1.271096247112533995, -9.720655361064800104, 1.999999999999998224 ) ) ;
#3136 = CARTESIAN_POINT ( 'NONE',  ( -7.375360291558941128, -1.341686286798741135, 1.999999999999998224 ) ) ;
#3137 = PRESENTATION_STYLE_ASSIGNMENT (( #2697 ) ) ;
#3138 = ADVANCED_FACE ( 'NONE', ( #3384 ), #1196, .T. ) ;
#3139 = PLANE ( 'NONE',  #4539 ) ;
#3140 =( NAMED_UNIT ( * ) SI_UNIT ( $, .STERADIAN. ) SOLID_ANGLE_UNIT ( ) );
#3141 = CARTESIAN_POINT ( 'NONE',  ( -3.110890340275366039, -5.031137978950550149, 1.999999999999998224 ) ) ;
#3142 = CARTESIAN_POINT ( 'NONE',  ( 5.526041665711819206, -0.8982374663919266977, 1.999999999999998224 ) ) ;
#3143 = DIRECTION ( 'NONE',  ( 0.9797958971132711969, 0.2000000000000000111, 0.000000000000000000 ) ) ;
#3144 = ORIENTED_EDGE ( 'NONE', *, *, #1806, .F. ) ;
#3145 = LINE ( 'NONE', #4405, #3191 ) ;
#3146 = CARTESIAN_POINT ( 'NONE',  ( -7.660583958272733973, 7.409732212661285011, 13.99999999999999645 ) ) ;
#3147 = ADVANCED_FACE ( 'NONE', ( #3925 ), #2975, .F. ) ;
#3148 =( NAMED_UNIT ( * ) SI_UNIT ( $, .STERADIAN. ) SOLID_ANGLE_UNIT ( ) );
#3149 = CARTESIAN_POINT ( 'NONE',  ( 21.75000000000000000, 2.891205793294679929E-17, 4.000000000000001776 ) ) ;
#3150 = EDGE_LOOP ( 'NONE', ( #874, #493 ) ) ;
#3151 = CARTESIAN_POINT ( 'NONE',  ( 1.300000000000000044, -1.082531754730548412, -0.6249999999999997780 ) ) ;
#3152 = CARTESIAN_POINT ( 'NONE',  ( 7.258279873954945671, -6.354128476750924293, 14.00000000000000000 ) ) ;
#3153 = CARTESIAN_POINT ( 'NONE',  ( 1.183015137239217474, -7.150809911821259135, 1.999999999999998224 ) ) ;
#3154 = ADVANCED_FACE ( 'NONE', ( #4356 ), #2945, .F. ) ;
#3155 = CARTESIAN_POINT ( 'NONE',  ( 7.716263785693136867, -3.801003699432787375, 1.999999999999998224 ) ) ;
#3156 = MECHANICAL_DESIGN_GEOMETRIC_PRESENTATION_REPRESENTATION (  '', ( #1583 ), #3882 ) ;
#3157 = CARTESIAN_POINT ( 'NONE',  ( 6.863489721961782308, 6.439594285166703180, 14.00000000000000000 ) ) ;
#3158 = VERTEX_POINT ( 'NONE', #410 ) ;
#3159 = CARTESIAN_POINT ( 'NONE',  ( -9.913420430684192652, 3.732070475089103834, 1.999999999999998224 ) ) ;
#3160 = CARTESIAN_POINT ( 'NONE',  ( -0.8169484412210609170, 6.196426872864405411, 14.00000000000000000 ) ) ;
#3161 = CARTESIAN_POINT ( 'NONE',  ( 5.381714297850043849, -6.137309488907495947, 13.99999999999999645 ) ) ;
#3162 = EDGE_CURVE ( 'NONE', #2517, #4073, #5564, .T. ) ;
#3163 = CARTESIAN_POINT ( 'NONE',  ( 7.565999024956893138, -2.848076369834590338, 13.99999999999999645 ) ) ;
#3164 = CARTESIAN_POINT ( 'NONE',  ( 5.326024957120313985, -1.813589758486611858, 14.00000000000000000 ) ) ;
#3165 = CARTESIAN_POINT ( 'NONE',  ( 8.454926800554316557, -3.338224220245900042, 1.999999999999998224 ) ) ;
#3166 = CYLINDRICAL_SURFACE ( 'NONE', #417, 27.00000000000000355 ) ;
#3167 = CIRCLE ( 'NONE', #2980, 25.00000000000000000 ) ;
#3168 = CARTESIAN_POINT ( 'NONE',  ( 18.00000000000000000, 1.553654299240552096E-15, -8.000000000000000000 ) ) ;
#3169 = DIRECTION ( 'NONE',  ( 1.000000000000000000, 0.000000000000000000, 0.000000000000000000 ) ) ;
#3170 = DIRECTION ( 'NONE',  ( 1.000000000000000000, 0.000000000000000000, 0.000000000000000000 ) ) ;
#3171=STYLED_ITEM('',(#5716),#4501);
#3172 = CARTESIAN_POINT ( 'NONE',  ( 2.200000000000000622, 0.000000000000000000, 0.000000000000000000 ) ) ;
#3173 = ADVANCED_FACE ( 'NONE', ( #2139 ), #3866, .T. ) ;
#3174 = AXIS2_PLACEMENT_3D ( 'NONE', #4054, #1863, #3621 ) ;
#3175 = CARTESIAN_POINT ( 'NONE',  ( 1.933011552319069404, 10.64041406927699640, 13.99999999999999645 ) ) ;
#3176 = DIRECTION ( 'NONE',  ( -3.540989467475305966E-16, -1.000000000000000000, 0.000000000000000000 ) ) ;
#3177 = ORIENTED_EDGE ( 'NONE', *, *, #1110, .T. ) ;
#3178 = ORIENTED_EDGE ( 'NONE', *, *, #4247, .T. ) ;
#3179 = CARTESIAN_POINT ( 'NONE',  ( -7.304208470128496167, 7.056621303512280896, 14.00000000000000000 ) ) ;
#3180 = CARTESIAN_POINT ( 'NONE',  ( 6.180183843827202317, 3.174252413088801461, 1.999999999999998224 ) ) ;
#3181 = VECTOR ( 'NONE', #2487, 1000.000000000000114 ) ;
#3182 = CARTESIAN_POINT ( 'NONE',  ( -7.425829140954076202, 3.215541426300492223, 1.999999999999998224 ) ) ;
#3183 = CARTESIAN_POINT ( 'NONE',  ( -6.681386044268952773, 6.252046474378028407, 14.00000000000000000 ) ) ;
#3184 = ORIENTED_EDGE ( 'NONE', *, *, #2209, .T. ) ;
#3185 = CARTESIAN_POINT ( 'NONE',  ( -4.581738566658409617, -9.288989786611782762, 1.999999999999998224 ) ) ;
#3186 = DIRECTION ( 'NONE',  ( 0.000000000000000000, 0.000000000000000000, -1.000000000000000000 ) ) ;
#3187 = CARTESIAN_POINT ( 'NONE',  ( 8.973806924230895987, -1.178693538871703250, 13.99999999999999645 ) ) ;
#3188 = AXIS2_PLACEMENT_3D ( 'NONE', #2361, #3257, #5008 ) ;
#3189 = CARTESIAN_POINT ( 'NONE',  ( 2.519353604429575011, -7.832629354751150963, 13.99999999999999645 ) ) ;
#3190 = CARTESIAN_POINT ( 'NONE',  ( -2.283612537812034216, 5.775797914528924437, 14.00000000000000000 ) ) ;
#3191 = VECTOR ( 'NONE', #1816, 1000.000000000000000 ) ;
#3192 = ORIENTED_EDGE ( 'NONE', *, *, #2134, .T. ) ;
#3193 = CARTESIAN_POINT ( 'NONE',  ( -5.921118896519414143, 6.318058289644735481, 1.999999999999998224 ) ) ;
#3194 = DIRECTION ( 'NONE',  ( 0.000000000000000000, 0.000000000000000000, 1.000000000000000000 ) ) ;
#3195 = ADVANCED_FACE ( 'NONE', ( #3842 ), #5594, .T. ) ;
#3196 = VECTOR ( 'NONE', #295, 1000.000000000000114 ) ;
#3197 = DIRECTION ( 'NONE',  ( 1.000000000000000000, 0.000000000000000000, 0.000000000000000000 ) ) ;
#3198 = FILL_AREA_STYLE_COLOUR ( '', #2593 ) ;
#3199 = CARTESIAN_POINT ( 'NONE',  ( -5.021280548121167975, 3.603657539922314967, 2.000000000001176392 ) ) ;
#3200 = ORIENTED_EDGE ( 'NONE', *, *, #4668, .T. ) ;
#3201 = CIRCLE ( 'NONE', #2826, 3.799999999999999378 ) ;
#3202 = CARTESIAN_POINT ( 'NONE',  ( -3.715337444063474770, -5.771435016728991840, 1.999999999999998224 ) ) ;
#3203 = LINE ( 'NONE', #4603, #1176 ) ;
#3204 = FILL_AREA_STYLE ('',( #3706 ) ) ;
#3205 = FACE_BOUND ( 'NONE', #907, .T. ) ;
#3206 = DIRECTION ( 'NONE',  ( -0.000000000000000000, -0.000000000000000000, 1.000000000000000000 ) ) ;
#3207 = EDGE_LOOP ( 'NONE', ( #3184, #4385 ) ) ;
#3208 = CARTESIAN_POINT ( 'NONE',  ( 0.000000000000000000, 0.000000000000000000, 4.000000000000000000 ) ) ;
#3209 = CARTESIAN_POINT ( 'NONE',  ( 9.320190601378300244, -2.164585516638619200, 14.00000000000000000 ) ) ;
#3210 = CARTESIAN_POINT ( 'NONE',  ( -5.402835942920797940, -5.063607225391133504, 1.999999999999998224 ) ) ;
#3211 = CARTESIAN_POINT ( 'NONE',  ( -6.667513054348624735, -4.302816426345351886, 1.999999999999998224 ) ) ;
#3212 = CARTESIAN_POINT ( 'NONE',  ( -9.772156678340820690, -2.119544458102511353, 14.00000000000000000 ) ) ;
#3213 = EDGE_LOOP ( 'NONE', ( #220, #2715, #1586, #1319 ) ) ;
#3214 = CARTESIAN_POINT ( 'NONE',  ( 5.800093669797941054, -8.375184749302256648, 1.999999999999998224 ) ) ;
#3215 = LINE ( 'NONE', #2754, #72 ) ;
#3216 = CARTESIAN_POINT ( 'NONE',  ( -8.388197440585694054, -1.387539741535495974, 13.99999999999999645 ) ) ;
#3217 = EDGE_CURVE ( 'NONE', #2170, #534, #5332, .T. ) ;
#3218 = CARTESIAN_POINT ( 'NONE',  ( -0.8169484412210609170, 6.196426872864405411, 14.00000000000000000 ) ) ;
#3219 = ORIENTED_EDGE ( 'NONE', *, *, #5235, .F. ) ;
#3220 = CARTESIAN_POINT ( 'NONE',  ( -7.884571930971327802, 3.418633173532902969, 1.999999999999998224 ) ) ;
#3221 = FACE_OUTER_BOUND ( 'NONE', #2706, .T. ) ;
#3222 = SURFACE_SIDE_STYLE ('',( #5057 ) ) ;
#3223 = CARTESIAN_POINT ( 'NONE',  ( -6.876639332705558161, 1.598006320995754237, 1.999999999999998224 ) ) ;
#3224 = EDGE_LOOP ( 'NONE', ( #4557, #1939, #4394, #2786 ) ) ;
#3225 = CARTESIAN_POINT ( 'NONE',  ( 7.439669587982602472, 0.9822684312230360870, 1.999999999999998224 ) ) ;
#3226 = CARTESIAN_POINT ( 'NONE',  ( 3.885274725274726393, -8.673617379884035472E-16, 0.000000000000000000 ) ) ;
#3227 = EDGE_CURVE ( 'NONE', #3499, #4303, #4549, .T. ) ;
#3228 = PLANE ( 'NONE',  #2068 ) ;
#3229 = CARTESIAN_POINT ( 'NONE',  ( 0.000000000000000000, 0.000000000000000000, 4.000000000000000000 ) ) ;
#3230 = ORIENTED_EDGE ( 'NONE', *, *, #3405, .T. ) ;
#3231 = DIRECTION ( 'NONE',  ( -0.000000000000000000, 0.000000000000000000, 1.000000000000000000 ) ) ;
#3232 = CARTESIAN_POINT ( 'NONE',  ( 1.124407659250215685, -9.699258357303232714, 14.00000000000000000 ) ) ;
#3233 = CARTESIAN_POINT ( 'NONE',  ( 5.857810772706377733, -5.665644577056675679, 1.999999999999998224 ) ) ;
#3234 = CARTESIAN_POINT ( 'NONE',  ( -7.588772809867561087, -4.728083520432016407, 1.999999999999998224 ) ) ;
#3235 = CARTESIAN_POINT ( 'NONE',  ( -9.986481889892992569, 1.144076113142371787, 14.00000000000000000 ) ) ;
#3236 = CARTESIAN_POINT ( 'NONE',  ( 23.48484848484848442, -8.570991287109677614, -8.000000000000000000 ) ) ;
#3237 = ORIENTED_EDGE ( 'NONE', *, *, #5526, .F. ) ;
#3238 = CARTESIAN_POINT ( 'NONE',  ( 1.380000000000002558, 21.95856267278071527, 15.94994774640597512 ) ) ;
#3239 = CARTESIAN_POINT ( 'NONE',  ( 1.300000000000000044, 0.000000000000000000, 0.000000000000000000 ) ) ;
#3240 = CARTESIAN_POINT ( 'NONE',  ( 1.598519525623709692, 9.677660462521252782, 13.99999999999999645 ) ) ;
#3241 = PRODUCT_RELATED_PRODUCT_CATEGORY ( 'part', '', ( #4227 ) ) ;
#3242 =( GEOMETRIC_REPRESENTATION_CONTEXT ( 3 ) GLOBAL_UNCERTAINTY_ASSIGNED_CONTEXT ( ( #2669 ) ) GLOBAL_UNIT_ASSIGNED_CONTEXT ( ( #946, #918, #431 ) ) REPRESENTATION_CONTEXT ( 'NONE', 'WORKASPACE' ) );
#3243 = CARTESIAN_POINT ( 'NONE',  ( 4.513069810084764377, -3.445129632735343339, 14.00000000000000000 ) ) ;
#3244 = VERTEX_POINT ( 'NONE', #63 ) ;
#3245 = CARTESIAN_POINT ( 'NONE',  ( 1.208067634251008604, -9.180948453718620783, 1.999999999999998224 ) ) ;
#3246 = DIRECTION ( 'NONE',  ( -1.000000000000000000, -0.000000000000000000, -0.000000000000000000 ) ) ;
#3247 =( NAMED_UNIT ( * ) PLANE_ANGLE_UNIT ( ) SI_UNIT ( $, .RADIAN. ) );
#3248 = CARTESIAN_POINT ( 'NONE',  ( -6.334648143026943679, -2.872559841353752308, 1.999999999999998224 ) ) ;
#3249 = ADVANCED_FACE ( 'NONE', ( #1821 ), #2769, .T. ) ;
#3250 = ORIENTED_EDGE ( 'NONE', *, *, #4431, .T. ) ;
#3251 = CARTESIAN_POINT ( 'NONE',  ( 7.097632634466812362, -2.668286824979932970, 1.999999999999998224 ) ) ;
#3252 = DIRECTION ( 'NONE',  ( 0.000000000000000000, 0.000000000000000000, -1.000000000000000000 ) ) ;
#3253 = SURFACE_STYLE_USAGE ( .BOTH. , #4091 ) ;
#3254 = FACE_OUTER_BOUND ( 'NONE', #673, .T. ) ;
#3255 = CIRCLE ( 'NONE', #2329, 1.610000000000000098 ) ;
#3256 = DIRECTION ( 'NONE',  ( 0.000000000000000000, 0.000000000000000000, 1.000000000000000000 ) ) ;
#3257 = DIRECTION ( 'NONE',  ( 0.000000000000000000, 0.000000000000000000, -1.000000000000000000 ) ) ;
#3258 = ORIENTED_EDGE ( 'NONE', *, *, #1286, .F. ) ;
#3259 = ADVANCED_FACE ( 'NONE', ( #3122 ), #4954, .T. ) ;
#3260 = CARTESIAN_POINT ( 'NONE',  ( 9.809999999999998721, 2.449293598294705921E-16, -1.999999999999999556 ) ) ;
#3261 = CARTESIAN_POINT ( 'NONE',  ( 5.030817567586885808, 9.062633982223131213, 14.00000000000000000 ) ) ;
#3262 = CARTESIAN_POINT ( 'NONE',  ( 8.952336951391263398, 1.032601321559316832, 1.999999999999998224 ) ) ;
#3263 = VECTOR ( 'NONE', #1205, 1000.000000000000000 ) ;
#3264 = CARTESIAN_POINT ( 'NONE',  ( -2.970508497641843881, 8.737606122598624125, 1.999999999999998224 ) ) ;
#3265 = CARTESIAN_POINT ( 'NONE',  ( 5.710084532570044225, 7.448680193042861220, 14.00000000000000000 ) ) ;
#3266=STYLED_ITEM('',(#5709),#2595);
#3267 = PLANE ( 'NONE',  #1892 ) ;
#3268 = ORIENTED_EDGE ( 'NONE', *, *, #3464, .F. ) ;
#3269 = FACE_OUTER_BOUND ( 'NONE', #1281, .T. ) ;
#3270 = CARTESIAN_POINT ( 'NONE',  ( 23.48484848484848442, -8.570991287109677614, 4.000000000000000000 ) ) ;
#3271 = CARTESIAN_POINT ( 'NONE',  ( 8.697835924490034287, 4.836984431370582982, 13.99999999999999645 ) ) ;
#3272 = VECTOR ( 'NONE', #1678, 1000.000000000000000 ) ;
#3273 = CARTESIAN_POINT ( 'NONE',  ( -3.987231204388229422, 4.693390172674912542, 13.99999999999953104 ) ) ;
#3274 = ORIENTED_EDGE ( 'NONE', *, *, #866, .F. ) ;
#3275 = CARTESIAN_POINT ( 'NONE',  ( -5.390757458300977412, 6.793134358447004750, 1.999999999999998224 ) ) ;
#3276 = DIRECTION ( 'NONE',  ( -1.000000000000000000, 0.000000000000000000, 0.000000000000000000 ) ) ;
#3277 = CLOSED_SHELL ( 'NONE', ( #1516, #251, #481, #3856, #2737, #1560, #5463, #4484, #3330, #1250, #1036, #2195, #1597, #196, #3779, #3423, #2455, #3619, #4843, #4825, #4194, #306, #1768 ) ) ;
#3278 = CIRCLE ( 'NONE', #1631, 4.500000000000000888 ) ;
#3279 = CARTESIAN_POINT ( 'NONE',  ( 4.815977876496239318, 4.225366587634176163, 1.999999999999998224 ) ) ;
#3280 = ORIENTED_EDGE ( 'NONE', *, *, #429, .F. ) ;
#3281 = CARTESIAN_POINT ( 'NONE',  ( -4.089163901200156381, 5.898691170885093982, 1.999999999999998224 ) ) ;
#3282 = CARTESIAN_POINT ( 'NONE',  ( 17.99999999999999289, -17.34935157289748631, -8.000000000000000000 ) ) ;
#3283 = VECTOR ( 'NONE', #4358, 1000.000000000000114 ) ;
#3284 = DIRECTION ( 'NONE',  ( -0.000000000000000000, -0.000000000000000000, 1.000000000000000000 ) ) ;
#3285 = AXIS2_PLACEMENT_3D ( 'NONE', #199, #2789, #1119 ) ;
#3286 = EDGE_CURVE ( 'NONE', #2170, #5417, #4648, .T. ) ;
#3287 = CARTESIAN_POINT ( 'NONE',  ( 0.000000000000000000, 0.000000000000000000, 2.000000000000000000 ) ) ;
#3288 = ORIENTED_EDGE ( 'NONE', *, *, #1667, .T. ) ;
#3289 = DIRECTION ( 'NONE',  ( -0.000000000000000000, -0.000000000000000000, 1.000000000000000000 ) ) ;
#3290 = CARTESIAN_POINT ( 'NONE',  ( 0.000000000000000000, 21.95856267278071527, 15.94994774640597512 ) ) ;
#3291 = EDGE_CURVE ( 'NONE', #2258, #2461, #972, .T. ) ;
#3292 = CARTESIAN_POINT ( 'NONE',  ( 6.401046915551857452, 6.194151307162986342, 1.999999999999998224 ) ) ;
#3293 = AXIS2_PLACEMENT_3D ( 'NONE', #3239, #995, #1830 ) ;
#3294 = CARTESIAN_POINT ( 'NONE',  ( 6.444084565535373343, 4.617298776321548281, 13.99999999999999645 ) ) ;
#3295 = CARTESIAN_POINT ( 'NONE',  ( 9.164356920907600568, 2.464151434936005192, 1.999999999999998224 ) ) ;
#3296 = CARTESIAN_POINT ( 'NONE',  ( -9.445900372710701376, 3.550092993115766760, 14.00000000000000000 ) ) ;
#3297 = ORIENTED_EDGE ( 'NONE', *, *, #4995, .T. ) ;
#3298 = DIRECTION ( 'NONE',  ( -4.364351673553916694E-15, 1.000000000000000000, 0.000000000000000000 ) ) ;
#3299 = EDGE_LOOP ( 'NONE', ( #5565, #241, #4404, #2201 ) ) ;
#3300 = CARTESIAN_POINT ( 'NONE',  ( 0.000000000000000000, 0.000000000000000000, 8.000000000000000000 ) ) ;
#3301 = CARTESIAN_POINT ( 'NONE',  ( -4.184906021401652687, -5.457255036755483069, 14.00000000000000000 ) ) ;
#3302 = CARTESIAN_POINT ( 'NONE',  ( 5.347643153870340171, -7.463670412150953837, 13.99999999999999645 ) ) ;
#3303 = CARTESIAN_POINT ( 'NONE',  ( 2.161943361801395014, -6.363123982928430067, 14.00000000000000000 ) ) ;
#3304 = ORIENTED_EDGE ( 'NONE', *, *, #2721, .T. ) ;
#3305 = CARTESIAN_POINT ( 'NONE',  ( -9.742306995815773973, -3.848972158781406083, 1.999999999999998224 ) ) ;
#3306 = PRODUCT_DEFINITION_SHAPE ( 'NONE', 'NONE',  #5209 ) ;
#3307 = DIRECTION ( 'NONE',  ( -1.000000000000000000, 0.000000000000000000, 0.000000000000000000 ) ) ;
#3308 = CARTESIAN_POINT ( 'NONE',  ( -2.189112655477410740, -6.464091385745793339, 1.999999999999998224 ) ) ;
#3309 = VERTEX_POINT ( 'NONE', #4926 ) ;
#3310 = CARTESIAN_POINT ( 'NONE',  ( 5.772253124442284111, -3.205917188174072230, 1.999999999999998224 ) ) ;
#3311 = CARTESIAN_POINT ( 'NONE',  ( 0.000000000000000000, 0.000000000000000000, 4.000000000000000000 ) ) ;
#3312 = DIRECTION ( 'NONE',  ( -1.000000000000000000, 0.000000000000000000, -0.000000000000000000 ) ) ;
#3313 = ADVANCED_FACE ( 'NONE', ( #10 ), #3578, .T. ) ;
#3314 = DIRECTION ( 'NONE',  ( -0.000000000000000000, -0.000000000000000000, -1.000000000000000000 ) ) ;
#3315 = UNCERTAINTY_MEASURE_WITH_UNIT (LENGTH_MEASURE( 1.000000000000000082E-05 ), #5388, 'distance_accuracy_value', 'NONE');
#3316 = DIRECTION ( 'NONE',  ( -1.000000000000000000, 0.000000000000000000, 0.000000000000000000 ) ) ;
#3317 = ORIENTED_EDGE ( 'NONE', *, *, #5186, .F. ) ;
#3318 = PLANE ( 'NONE',  #3828 ) ;
#3319 = CYLINDRICAL_SURFACE ( 'NONE', #3359, 12.50000000000000000 ) ;
#3320 = CARTESIAN_POINT ( 'NONE',  ( -0.3010823416051299772, -9.281161307073867661, 1.999999999999998224 ) ) ;
#3321 = EDGE_CURVE ( 'NONE', #4851, #899, #577, .T. ) ;
#3322 = CARTESIAN_POINT ( 'NONE',  ( -3.594774944545354955, 7.935102286574237773, 13.99999999999999645 ) ) ;
#3323 = CARTESIAN_POINT ( 'NONE',  ( 10.50003631213658117, 0.006025845833179007717, 14.00000000000000000 ) ) ;
#3324 = VERTEX_POINT ( 'NONE', #2657 ) ;
#3325 = FACE_BOUND ( 'NONE', #3385, .T. ) ;
#3326 = EDGE_LOOP ( 'NONE', ( #1197, #987, #3483 ) ) ;
#3327 = CARTESIAN_POINT ( 'NONE',  ( 10.40193138080405255, 3.529992181067783452, 1.999999999999998224 ) ) ;
#3328 = CARTESIAN_POINT ( 'NONE',  ( 7.280083392764700179, -2.072676875633882254, 14.00000000000000000 ) ) ;
#3329 = CARTESIAN_POINT ( 'NONE',  ( -8.402144917908875854, 4.670158400850172420, 13.99999999999999645 ) ) ;
#3330 = ADVANCED_FACE ( 'NONE', ( #5277 ), #985, .F. ) ;
#3331 = CARTESIAN_POINT ( 'NONE',  ( -1.987635485262058577, 6.951293809708866789, 14.00000000000000000 ) ) ;
#3332 = ORIENTED_EDGE ( 'NONE', *, *, #412, .T. ) ;
#3333 = CARTESIAN_POINT ( 'NONE',  ( -7.945634105012028492, -6.745245841440164369, 1.999999999999998224 ) ) ;
#3334 = ADVANCED_FACE ( 'NONE', ( #3546 ), #4870, .F. ) ;
#3335 = LINE ( 'NONE', #2988, #4368 ) ;
#3336 = CARTESIAN_POINT ( 'NONE',  ( 0.000000000000000000, 0.000000000000000000, 0.000000000000000000 ) ) ;
#3337 = CARTESIAN_POINT ( 'NONE',  ( -5.395431796987671724, -5.765308706272893602, 1.999999999999998224 ) ) ;
#3338 = ORIENTED_EDGE ( 'NONE', *, *, #3071, .F. ) ;
#3339 = CARTESIAN_POINT ( 'NONE',  ( -2.020383375745208987, -7.552201994671270846, 1.999999999999998224 ) ) ;
#3340 = CARTESIAN_POINT ( 'NONE',  ( -0.4015567206217142693, -6.330257989742454683, 1.999999999999998224 ) ) ;
#3341 = CARTESIAN_POINT ( 'NONE',  ( 3.426039378954557346, 5.938690629332270987, 13.99999999999999645 ) ) ;
#3342 = CARTESIAN_POINT ( 'NONE',  ( -1.380000000000054960, 3.291637795666119257E-15, 4.000000000000000000 ) ) ;
#3343 = VECTOR ( 'NONE', #1330, 1000.000000000000000 ) ;
#3344 = FACE_OUTER_BOUND ( 'NONE', #3326, .T. ) ;
#3345 = EDGE_LOOP ( 'NONE', ( #4975, #5250, #1541, #5450 ) ) ;
#3346 = DIRECTION ( 'NONE',  ( 1.000000000000000000, 0.000000000000000000, 0.000000000000000000 ) ) ;
#3347 = DIRECTION ( 'NONE',  ( 1.000000000000000000, 0.000000000000000000, 0.000000000000000000 ) ) ;
#3348 = CARTESIAN_POINT ( 'NONE',  ( -1.484422800923325125, -8.172499773499277254, 1.999999999999998224 ) ) ;
#3349 = CIRCLE ( 'NONE', #4633, 5.000000000000000000 ) ;
#3350 = CARTESIAN_POINT ( 'NONE',  ( 7.132151089625189400, 3.519983721611798622, 13.99999999999999645 ) ) ;
#3351 = LINE ( 'NONE', #1999, #303 ) ;
#3352 = ORIENTED_EDGE ( 'NONE', *, *, #1716, .T. ) ;
#3353 = DIRECTION ( 'NONE',  ( 0.000000000000000000, 0.000000000000000000, -1.000000000000000000 ) ) ;
#3354 = ORIENTED_EDGE ( 'NONE', *, *, #788, .T. ) ;
#3355 = LINE ( 'NONE', #4220, #2456 ) ;
#3356 = AXIS2_PLACEMENT_3D ( 'NONE', #2520, #4284, #2094 ) ;
#3357 = CARTESIAN_POINT ( 'NONE',  ( 7.097632634466814139, -2.668286824980076855, 14.00000000000000000 ) ) ;
#3358 = CARTESIAN_POINT ( 'NONE',  ( -5.250997584835957355, 8.145342823909338392, 13.99999999999999645 ) ) ;
#3359 = AXIS2_PLACEMENT_3D ( 'NONE', #5444, #1498, #2882 ) ;
#3360 =( GEOMETRIC_REPRESENTATION_CONTEXT ( 3 ) GLOBAL_UNCERTAINTY_ASSIGNED_CONTEXT ( ( #4179 ) ) GLOBAL_UNIT_ASSIGNED_CONTEXT ( ( #310, #1183, #834 ) ) REPRESENTATION_CONTEXT ( 'NONE', 'WORKASPACE' ) );
#3361 = CARTESIAN_POINT ( 'NONE',  ( 4.815977876496241095, 4.225366587634054483, 14.00000000000000000 ) ) ;
#3362 = ORIENTED_EDGE ( 'NONE', *, *, #3752, .F. ) ;
#3363 = CARTESIAN_POINT ( 'NONE',  ( 6.019515613300546519, 7.843576796802394391, 1.999999999999998224 ) ) ;
#3364 = CIRCLE ( 'NONE', #2904, 23.00000000000000000 ) ;
#3365 = DIRECTION ( 'NONE',  ( -0.000000000000000000, -0.000000000000000000, 1.000000000000000000 ) ) ;
#3366 = DIRECTION ( 'NONE',  ( 1.000000000000000000, 0.000000000000000000, 0.000000000000000000 ) ) ;
#3367 = CARTESIAN_POINT ( 'NONE',  ( -6.453089103408601090, 4.947336467533990145, 1.999999999999998224 ) ) ;
#3368 = VECTOR ( 'NONE', #91, 1000.000000000000000 ) ;
#3369 = CARTESIAN_POINT ( 'NONE',  ( 6.026041665150464688, -0.9817477132364114123, 1.999999999999998224 ) ) ;
#3370 = CARTESIAN_POINT ( 'NONE',  ( -0.8811140424828162176, 6.693995663234412419, 13.99999999999999645 ) ) ;
#3371 = CIRCLE ( 'NONE', #1715, 22.50000000000000355 ) ;
#3372 =( LENGTH_UNIT ( ) NAMED_UNIT ( * ) SI_UNIT ( .MILLI., .METRE. ) );
#3373 =( GEOMETRIC_REPRESENTATION_CONTEXT ( 3 ) GLOBAL_UNCERTAINTY_ASSIGNED_CONTEXT ( ( #2708 ) ) GLOBAL_UNIT_ASSIGNED_CONTEXT ( ( #5247, #923, #4432 ) ) REPRESENTATION_CONTEXT ( 'NONE', 'WORKASPACE' ) );
#3374 = CARTESIAN_POINT ( 'NONE',  ( 1.300000000000000044, -0.7216878364870318308, 1.249999999999999778 ) ) ;
#3375 = FACE_OUTER_BOUND ( 'NONE', #4645, .T. ) ;
#3376 = ORIENTED_EDGE ( 'NONE', *, *, #624, .T. ) ;
#3377 = FACE_OUTER_BOUND ( 'NONE', #2230, .T. ) ;
#3378 = DIRECTION ( 'NONE',  ( 0.000000000000000000, -1.000000000000000000, -0.000000000000000000 ) ) ;
#3379 = CARTESIAN_POINT ( 'NONE',  ( -9.406456921418630657, 1.708717176649225511, 1.999999999999998224 ) ) ;
#3380 = VECTOR ( 'NONE', #4175, 1000.000000000000000 ) ;
#3381 = CARTESIAN_POINT ( 'NONE',  ( 9.077580196901687160, 4.112174628513754371, 13.99999999999999645 ) ) ;
#3382 = DIRECTION ( 'NONE',  ( -1.000000000000000000, 0.000000000000000000, -0.000000000000000000 ) ) ;
#3383 = ORIENTED_EDGE ( 'NONE', *, *, #4034, .T. ) ;
#3384 = FACE_OUTER_BOUND ( 'NONE', #4966, .T. ) ;
#3385 = EDGE_LOOP ( 'NONE', ( #3524, #640 ) ) ;
#3386 = VECTOR ( 'NONE', #5061, 1000.000000000000000 ) ;
#3387 = DIRECTION ( 'NONE',  ( -4.364351673553916694E-15, 1.000000000000000000, 0.000000000000000000 ) ) ;
#3388 = CARTESIAN_POINT ( 'NONE',  ( 6.523553822664519330, -0.1051741892335816969, 14.00000000000000000 ) ) ;
#3389 = CARTESIAN_POINT ( 'NONE',  ( -4.310533329768688304, 5.077046166951620698, 1.999999999999412914 ) ) ;
#3390 = CARTESIAN_POINT ( 'NONE',  ( -5.034899347480884302, -4.722558430572732391, 14.00000000000000000 ) ) ;
#3391 = EDGE_CURVE ( 'NONE', #2508, #2807, #4464, .T. ) ;
#3392 = ORIENTED_EDGE ( 'NONE', *, *, #679, .F. ) ;
#3393 = CARTESIAN_POINT ( 'NONE',  ( 8.595497693523489247, -5.345940745659027549, 1.999999999999998224 ) ) ;
#3394 = EDGE_CURVE ( 'NONE', #5130, #760, #3631, .T. ) ;
#3395 = LINE ( 'NONE', #5147, #3263 ) ;
#3396 = CARTESIAN_POINT ( 'NONE',  ( 6.592258996018686368, -3.799026305082465971, 1.999999999999998224 ) ) ;
#3397 = DIRECTION ( 'NONE',  ( -0.000000000000000000, -0.000000000000000000, 1.000000000000000000 ) ) ;
#3398 = CARTESIAN_POINT ( 'NONE',  ( -2.721086536275892254, 7.222755814214462333, 13.99999999999999645 ) ) ;
#3399 = B_SPLINE_SURFACE_WITH_KNOTS ( 'NONE', 1, 3, ( 
 ( #1752, #5296, #1356, #919, #4427, #482, #2241, #1811, #3570, #3141, #4888, #2270, #3654, #1865, #5462, #1519, #3199, #2848, #1087, #4117, #3622, #170, #4969, #2785, #5381, #1116, #226, #5408, #2873, #4570, #3279, #1466, #4946, #631, #2295, #4055, #5031, #2819, #1004, #1439, #5493, #2763, #2382, #1488, #4141, #4626, #566, #4600, #1555, #108, #600, #3308, #4515, #2322, #1980, #4171, #4084, #3677, #3248, #195, #5058, #137, #1896, #3223, #1027, #2409, #4541, #2350, #1922, #3735, #659, #5433, #4997, #1057, #1948, #3702, #4202, #2066, #3853, #2440, #5579, #1640, #3766, #253, #5520, #2556, #1207, #1180, #2931, #5171, #366, #3396, #3878, #3793, #4229, #688, #1578, #2495, #3445, #5633, #1690, #4656, #4317, #5149, #5204, #2124, #3337, #1145, #2471, #4683, #2095, #1263, #3823, #3025, #2012, #280, #2959, #4708, #3367, #5088, #4254, #771, #2903, #1232, #722, #2037, #5550, #1607, #5122, #743, #2521, #4285, #339, #305, #5605, #1664, #3420, #2991, #4737, #803, #2645, #3531, #49, #2264, #3591, #3080, #4023, #3906, #3476, #2694, #939, #5663, #453, #22, #913, #79, #2153, #2582, #425, #4341, #4883, #2183, #5263, #392, #508, #1804, #4450, #1834, #885, #5344, #1724, #5238, #2212, #2234, #830, #3963, #1775, #1294, #3051, #4795, #1402, #5292, #1318, #4824, #3563, #4769, #1349, #856, #3938, #2612, #4371, #2415, #4398, #1748, #3503, #3109, #4857, #2671, #4423, #476, #3990, #5320, #1379, #3135, #3646, #4562, #218, #592, #1975, #1081, #2757, #4535, #5429, #131, #3728, #4965, #2344, #4912, #3697, #2843, #1861, #970, #4510, #4595, #654, #4110, #1918, #164, #2404, #3673, #626, #2317, #4941, #5487, #1461, #1023, #1484, #2376, #4136, #4050, #5455, #1944 ),
 ( #4165, #562, #3164, #3243, #191, #4077, #104, #4990, #2728, #4481, #1511, #1050, #3617, #539, #2290, #5375, #2811, #3273, #5024, #1431, #3190, #999, #3218, #2781, #1890, #5403, #765, #2434, #2090, #332, #3361, #1111, #5115, #4223, #2033, #4621, #361, #5166, #2897, #2117, #3818, #2515, #716, #4196, #5572, #1549, #3303, #4280, #2057, #245, #2868, #4731, #2007, #1632, #738, #3390, #3873, #5515, #3848, #796, #5053, #5543, #2549, #680, #3759, #1227, #3414, #1574, #2925, #2492, #5142, #4310, #3331, #5082, #4649, #1137, #1659, #2466, #3788, #275, #2983, #5600, #1600, #1171, #4677, #4248, #299, #1201, #2951, #4703, #1684, #4816, #879, #3018, #3440, #4763, #1798, #448, #419, #2177, #4416, #5313, #2638, #3128, #3044, #3471, #5625, #824, #1743, #2687, #4877, #933, #3900, #3553, #4392, #4443, #1373, #2577, #386, #1718, #3933, #1341, #498, #3072, #2257, #5198, #5232, #1313, #2205, #2605, #1257, #3498, #3957, #4335, #470, #2146, #5657, #1289, #4789, #849, #4363, #16, #1767, #3523, #5685, #5285, #3101, #5257, #4849, #906, #2665, #2229, #3982, #42, #4014, #2836, #4933, #98, #2283, #3691, #2337, #4043, #584, #1854, #992, #5448, #2370, #4103, #3611, #1424, #3183, #4588, #157, #4130, #1478, #5422, #1882, #71, #1456, #1396, #4960, #1502, #3265, #3157, #963, #1913, #1827, #2720, #5016, #1074, #3585, #646, #1042, #616, #3668, #184, #4903, #5338, #1017, #4503, #5366, #2751, #1937, #2803, #556, #4472, #2311, #4071, #532, #123, #3640, #4555, #5396, #3212, #2775, #4530, #3235, #4983, #3296, #2973, #2484, #2507, #5563, #3780, #4240, #2049, #3807, #5159, #3407, #1129, #1591, #2860, #266, #1219, #5592, #4186, #321, #1652, #291, #1193, #1624, #3323 ) ),
 .UNSPECIFIED., .F., .F., .F.,
 ( 2, 2 ),
 ( 4, 2, 2, 2, 2, 2, 2, 2, 2, 2, 2, 2, 2, 2, 2, 2, 2, 2, 2, 2, 2, 2, 2, 2, 2, 2, 2, 2, 2, 2, 2, 2, 2, 2, 2, 2, 2, 2, 2, 2, 2, 2, 2, 2, 2, 2, 2, 2, 2, 2, 2, 2, 2, 2, 2, 2, 2, 2, 2, 2, 2, 2, 2, 2, 2, 2, 2, 2, 2, 2, 2, 2, 2, 2, 2, 2, 2, 2, 2, 2, 2, 2, 2, 2, 2, 2, 2, 2, 2, 2, 2, 2, 2, 2, 2, 2, 2, 2, 2, 2, 2, 2, 2, 2, 2, 2, 2, 2, 2, 2, 2, 2, 2, 2, 2, 2, 2, 2, 2, 2, 4 ),
 ( 0.5000000000000000000, 0.9800000000000000933 ),
 ( 0.000000000000000000, 0.01562500000000000000, 0.03125000000000000000, 0.04687500000000000000, 0.06250000000000000000, 0.07812500000000000000, 0.09375000000000000000, 0.1093750000000000000, 0.1250000000000000000, 0.1328125000000000000, 0.1406250000000000000, 0.1484375000000000000, 0.1562500000000000000, 0.1640625000000000000, 0.1718750000000000000, 0.1796875000000000000, 0.1875000000000000000, 0.1953125000000000000, 0.2031250000000000000, 0.2109375000000000000, 0.2187500000000000000, 0.2265625000000000000, 0.2343750000000000000, 0.2421875000000000000, 0.2500000000000000000, 0.2578125000000000000, 0.2656250000000000000, 0.2734375000000000000, 0.2812500000000000000, 0.2890625000000000000, 0.2968750000000000000, 0.3046875000000000000, 0.3125000000000000000, 0.3203125000000000000, 0.3281250000000000000, 0.3359375000000000000, 0.3437500000000000000, 0.3515625000000000000, 0.3593750000000000000, 0.3671875000000000000, 0.3750000000000000000, 0.3828125000000000000, 0.3906250000000000000, 0.3984375000000000000, 0.4062500000000000000, 0.4140625000000000000, 0.4218750000000000000, 0.4296875000000000000, 0.4375000000000000000, 0.4453125000000000000, 0.4531250000000000000, 0.4609375000000000000, 0.4687500000000000000, 0.4765625000000000000, 0.4843750000000000000, 0.4921875000000000000, 0.5000000000000000000, 0.5078125000000000000, 0.5156250000000000000, 0.5234375000000000000, 0.5312500000000000000, 0.5390625000000000000, 0.5468750000000000000, 0.5546875000000000000, 0.5625000000000000000, 0.5703125000000000000, 0.5781250000000000000, 0.5859375000000000000, 0.5937500000000000000, 0.6015625000000000000, 0.6093750000000000000, 0.6171875000000000000, 0.6250000000000000000, 0.6328125000000000000, 0.6406250000000000000, 0.6484375000000000000, 0.6562500000000000000, 0.6640625000000000000, 0.6718750000000000000, 0.6796875000000000000, 0.6875000000000000000, 0.6953125000000000000, 0.7031250000000000000, 0.7109375000000000000, 0.7187500000000000000, 0.7265625000000000000, 0.7343750000000000000, 0.7421875000000000000, 0.7500000000000000000, 0.7578125000000000000, 0.7656250000000000000, 0.7734375000000000000, 0.7812500000000000000, 0.7890625000000000000, 0.7968750000000000000, 0.8046875000000000000, 0.8125000000000000000, 0.8203125000000000000, 0.8281250000000000000, 0.8359375000000000000, 0.8437500000000000000, 0.8515625000000000000, 0.8593750000000000000, 0.8671875000000000000, 0.8750000000000000000, 0.8828125000000000000, 0.8906250000000000000, 0.8984375000000000000, 0.9062500000000000000, 0.9140625000000000000, 0.9218750000000000000, 0.9296875000000000000, 0.9375000000000000000, 0.9453125000000000000, 0.9531250000000000000, 0.9609375000000000000, 0.9687500000000000000, 0.9765625000000000000, 0.9843750000000000000, 0.9921875000000000000, 1.000000000000000000 ),
 .UNSPECIFIED. ) ;
#3400 = CARTESIAN_POINT ( 'NONE',  ( 7.379526280503348801, 5.862399640741291051, 1.999999999999998224 ) ) ;
#3401 = PLANE ( 'NONE',  #5477 ) ;
#3402 = EDGE_LOOP ( 'NONE', ( #37, #3641 ) ) ;
#3403 = CARTESIAN_POINT ( 'NONE',  ( 0.000000000000000000, 0.000000000000000000, 14.00000000000000000 ) ) ;
#3404 = DIRECTION ( 'NONE',  ( 0.000000000000000000, 0.000000000000000000, -1.000000000000000000 ) ) ;
#3405 = EDGE_CURVE ( 'NONE', #5130, #4697, #491, .T. ) ;
#3406 = CARTESIAN_POINT ( 'NONE',  ( -0.1462562576243747192, 8.775315755192165668, 13.99999999999999645 ) ) ;
#3407 = CARTESIAN_POINT ( 'NONE',  ( 0.1634456542307747284, 10.28566380800474889, 14.00000000000000000 ) ) ;
#3408 = ORIENTED_EDGE ( 'NONE', *, *, #3796, .F. ) ;
#3409 = CARTESIAN_POINT ( 'NONE',  ( 17.74999999999999289, -15.01665741768121443, 4.000000000000000000 ) ) ;
#3410 = ORIENTED_EDGE ( 'NONE', *, *, #2354, .T. ) ;
#3411 = CARTESIAN_POINT ( 'NONE',  ( 0.000000000000000000, 0.000000000000000000, 4.000000000000003553 ) ) ;
#3412 = CARTESIAN_POINT ( 'NONE',  ( -5.416162817796315920, -4.301262981183149314, 14.00000000000000000 ) ) ;
#3413 = CARTESIAN_POINT ( 'NONE',  ( -4.892757975385814362, 9.527326283048992650, 13.99999999999999645 ) ) ;
#3414 = CARTESIAN_POINT ( 'NONE',  ( -6.041022033915573353, 3.753782041847178341, 14.00000000000000000 ) ) ;
#3415 = ORIENTED_EDGE ( 'NONE', *, *, #3073, .T. ) ;
#3416 = EDGE_CURVE ( 'NONE', #5658, #5339, #2712, .T. ) ;
#3417 = CARTESIAN_POINT ( 'NONE',  ( -7.551678268146208239, 5.989845445213456188, 1.999999999999998224 ) ) ;
#3418 = DIRECTION ( 'NONE',  ( 0.000000000000000000, 0.000000000000000000, -1.000000000000000000 ) ) ;
#3419 =( LENGTH_UNIT ( ) NAMED_UNIT ( * ) SI_UNIT ( .MILLI., .METRE. ) );
#3420 = CARTESIAN_POINT ( 'NONE',  ( 8.156937663705429387, 2.333191796391003603, 1.999999999999998224 ) ) ;
#3421 = CARTESIAN_POINT ( 'NONE',  ( -6.576488680450179203, -0.2289623203888876135, 1.999999999999998224 ) ) ;
#3422 = CARTESIAN_POINT ( 'NONE',  ( 6.638644669766899931, 2.135480210976827831, 13.99999999999999645 ) ) ;
#3423 = ADVANCED_FACE ( 'NONE', ( #4465 ), #524, .F. ) ;
#3424 = CARTESIAN_POINT ( 'NONE',  ( -2.331745755519268215, 9.978964459600444314, 1.999999999999998224 ) ) ;
#3425 = DIRECTION ( 'NONE',  ( -0.000000000000000000, -0.000000000000000000, 1.000000000000000000 ) ) ;
#3426 = VERTEX_POINT ( 'NONE', #2745 ) ;
#3427 = DIRECTION ( 'NONE',  ( -1.000000000000000000, 0.000000000000000000, 0.000000000000000000 ) ) ;
#3428 = AXIS2_PLACEMENT_3D ( 'NONE', #4736, #1179, #5519 ) ;
#3429 = DIRECTION ( 'NONE',  ( 0.000000000000000000, 0.000000000000000000, 1.000000000000000000 ) ) ;
#3430 = CARTESIAN_POINT ( 'NONE',  ( 1.208067634251009270, -9.180948453718622559, 13.99999999999999645 ) ) ;
#3431 = LINE ( 'NONE', #353, #5274 ) ;
#3432 = EDGE_LOOP ( 'NONE', ( #2451, #420 ) ) ;
#3433 = DIRECTION ( 'NONE',  ( -0.000000000000000000, -0.000000000000000000, 1.000000000000000000 ) ) ;
#3434 = EDGE_LOOP ( 'NONE', ( #1575, #843, #4249, #2252 ) ) ;
#3435 = CARTESIAN_POINT ( 'NONE',  ( 0.000000000000000000, 0.000000000000000000, 4.000000000000000000 ) ) ;
#3436 = CARTESIAN_POINT ( 'NONE',  ( -5.395431796987672612, -5.765308706272596950, 14.00000000000000000 ) ) ;
#3437 = CARTESIAN_POINT ( 'NONE',  ( -10.17357856257779680, 2.902115915870757679, 13.99999999999999645 ) ) ;
#3438 = PRODUCT_DEFINITION_CONTEXT ( 'detailed design', #2662, 'design' ) ;
#3439 = DIRECTION ( 'NONE',  ( -1.000000000000000000, -0.000000000000000000, -0.000000000000000000 ) ) ;
#3440 = CARTESIAN_POINT ( 'NONE',  ( 5.053476174606819527, -5.757900651972699180, 14.00000000000000000 ) ) ;
#3441 = VECTOR ( 'NONE', #889, 1000.000000000000000 ) ;
#3442 = VERTEX_POINT ( 'NONE', #550 ) ;
#3443 = CARTESIAN_POINT ( 'NONE',  ( -9.913420430684192652, 3.732070475089103834, 1.999999999999998224 ) ) ;
#3444 = CARTESIAN_POINT ( 'NONE',  ( 6.460119401626726265, -2.924461030940389783, 13.99999999999999645 ) ) ;
#3445 = CARTESIAN_POINT ( 'NONE',  ( 1.760389272475360256, -7.536528230137968798, 1.999999999999998224 ) ) ;
#3446 = CYLINDRICAL_SURFACE ( 'NONE', #720, 13.00000000000000178 ) ;
#3447 = CARTESIAN_POINT ( 'NONE',  ( -5.322107489685387272, 5.499660323246577498, 13.99999999999999645 ) ) ;
#3448 = CARTESIAN_POINT ( 'NONE',  ( -997.9783121635130101, 0.000000000000000000, 0.000000000000000000 ) ) ;
#3449 = AXIS2_PLACEMENT_3D ( 'NONE', #1011, #2222, #1875 ) ;
#3450 = SURFACE_STYLE_FILL_AREA ( #746 ) ;
#3451 = CARTESIAN_POINT ( 'NONE',  ( 0.3244988297792679166, -9.772062696132405080, 1.999999999999998224 ) ) ;
#3452 = PLANE ( 'NONE',  #3919 ) ;
#3453 = DIRECTION ( 'NONE',  ( 0.000000000000000000, 0.000000000000000000, 1.000000000000000000 ) ) ;
#3454 = ORIENTED_EDGE ( 'NONE', *, *, #3022, .F. ) ;
#3455 = VECTOR ( 'NONE', #4663, 1000.000000000000000 ) ;
#3456 = DIRECTION ( 'NONE',  ( -1.000000000000000000, 0.000000000000000000, 0.000000000000000000 ) ) ;
#3457 = DIRECTION ( 'NONE',  ( -1.000000000000000000, 3.540989467475305966E-16, 0.000000000000000000 ) ) ;
#3458 = CARTESIAN_POINT ( 'NONE',  ( 5.348203032363755050, 8.300083771889282147, 13.99999999999999645 ) ) ;
#3459 = EDGE_CURVE ( 'NONE', #1815, #3309, #2304, .T. ) ;
#3460 = CIRCLE ( 'NONE', #1443, 1.899999999999999689 ) ;
#3461 = CARTESIAN_POINT ( 'NONE',  ( 6.000000000000000000, 0.000000000000000000, 1.999999999999998224 ) ) ;
#3462 = VERTEX_POINT ( 'NONE', #1067 ) ;
#3463 = DIRECTION ( 'NONE',  ( 0.000000000000000000, 0.000000000000000000, 1.000000000000000000 ) ) ;
#3464 = EDGE_CURVE ( 'NONE', #4488, #1655, #4198, .T. ) ;
#3465 = ORIENTED_EDGE ( 'NONE', *, *, #2228, .T. ) ;
#3466 = DIRECTION ( 'NONE',  ( 0.000000000000000000, 0.000000000000000000, -1.000000000000000000 ) ) ;
#3467 = CARTESIAN_POINT ( 'NONE',  ( 3.857245400775171529, -7.804869966781184054, 14.00000000000000000 ) ) ;
#3468 = CARTESIAN_POINT ( 'NONE',  ( 4.243312049792013596, -4.537448458213932945, 1.999999999999998224 ) ) ;
#3469 = VECTOR ( 'NONE', #1711, 1000.000000000000000 ) ;
#3470 = LINE ( 'NONE', #905, #2795 ) ;
#3471 = CARTESIAN_POINT ( 'NONE',  ( -4.895455514773497718, -6.178604150901620073, 14.00000000000000000 ) ) ;
#3472 = AXIS2_PLACEMENT_3D ( 'NONE', #4574, #634, #2385 ) ;
#3473 = VERTEX_POINT ( 'NONE', #3772 ) ;
#3474 = FACE_BOUND ( 'NONE', #1867, .T. ) ;
#3475 = CARTESIAN_POINT ( 'NONE',  ( 2.406079317367887604, 6.392288322179703108, 13.99999999999999645 ) ) ;
#3476 = CARTESIAN_POINT ( 'NONE',  ( 3.208073253695059801, -8.107602109809695534, 1.999999999999998224 ) ) ;
#3477 = CARTESIAN_POINT ( 'NONE',  ( 7.992346231215205599, -0.9198489573344823533, 1.999999999999998224 ) ) ;
#3478 = CARTESIAN_POINT ( 'NONE',  ( -4.227552200850896114, 7.601683304540504338, 13.99999999999999645 ) ) ;
#3479 = DIRECTION ( 'NONE',  ( -0.000000000000000000, -0.000000000000000000, 1.000000000000000000 ) ) ;
#3480 = LINE ( 'NONE', #3597, #3707 ) ;
#3481 = LINE ( 'NONE', #2100, #4553 ) ;
#3482 = DIRECTION ( 'NONE',  ( 0.000000000000000000, 0.000000000000000000, 1.000000000000000000 ) ) ;
#3483 = ORIENTED_EDGE ( 'NONE', *, *, #3391, .F. ) ;
#3484 = LINE ( 'NONE', #3574, #5486 ) ;
#3485 = EDGE_CURVE ( 'NONE', #4336, #4516, #203, .T. ) ;
#3486 = CARTESIAN_POINT ( 'NONE',  ( -3.290073422422831406, -8.739709727799914063, 13.99999999999999645 ) ) ;
#3487 = SHAPE_REPRESENTATION ( 'outer cover 1', ( #1336 ), #2338 ) ;
#3488 = CARTESIAN_POINT ( 'NONE',  ( 1.300000000000000044, -1.443375672974063884, -3.691112476943992763E-18 ) ) ;
#3489 = EDGE_LOOP ( 'NONE', ( #5345, #64, #460, #17, #557 ) ) ;
#3490 = PRODUCT_DEFINITION_SHAPE ( 'NONE', 'NONE',  #5689 ) ;
#3491 = CARTESIAN_POINT ( 'NONE',  ( 0.000000000000000000, 0.000000000000000000, 0.000000000000000000 ) ) ;
#3492 = ORIENTED_EDGE ( 'NONE', *, *, #4154, .F. ) ;
#3493 = CARTESIAN_POINT ( 'NONE',  ( 25.00000000000000000, -3.061616997868383043E-15, 0.000000000000000000 ) ) ;
#3494 = CARTESIAN_POINT ( 'NONE',  ( 8.518575158374426692, 0.2826087140540691767, 14.00000000000000000 ) ) ;
#3495 = ADVANCED_FACE ( 'NONE', ( #1495 ), #1034, .T. ) ;
#3496 = CARTESIAN_POINT ( 'NONE',  ( 1.933011552319069404, 10.64041406927699640, 13.99999999999999645 ) ) ;
#3497 = DIRECTION ( 'NONE',  ( -4.364351673553916694E-15, 1.000000000000000000, 0.000000000000000000 ) ) ;
#3498 = CARTESIAN_POINT ( 'NONE',  ( 5.528193227149303723, 6.314447692498919018, 14.00000000000000000 ) ) ;
#3499 = VERTEX_POINT ( 'NONE', #4580 ) ;
#3500 = DIRECTION ( 'NONE',  ( 0.000000000000000000, 0.000000000000000000, -1.000000000000000000 ) ) ;
#3501 = CARTESIAN_POINT ( 'NONE',  ( -4.256527737016168267, -4.845957569453232416, 13.99999999999999645 ) ) ;
#3502 = SHAPE_DEFINITION_REPRESENTATION ( #1966, #1362 ) ;
#3503 = CARTESIAN_POINT ( 'NONE',  ( 8.172274133037948474, -5.076547540501181288, 1.999999999999998224 ) ) ;
#3504 = EDGE_CURVE ( 'NONE', #760, #3984, #2828, .T. ) ;
#3505 = CARTESIAN_POINT ( 'NONE',  ( -5.745624475482103755, 5.035517847229626476, 1.999999999999998224 ) ) ;
#3506 = CARTESIAN_POINT ( 'NONE',  ( 23.00000000000000000, -2.168404344971008868E-16, 4.000000000000000000 ) ) ;
#3507 = DIRECTION ( 'NONE',  ( 0.000000000000000000, 0.000000000000000000, 1.000000000000000000 ) ) ;
#3508 = DIRECTION ( 'NONE',  ( 0.000000000000000000, 1.000000000000000000, 0.000000000000000000 ) ) ;
#3509 = DIRECTION ( 'NONE',  ( -1.000000000000000000, 1.224646799147353207E-16, 0.000000000000000000 ) ) ;
#3510 = DIRECTION ( 'NONE',  ( 1.000000000000000000, 0.000000000000000000, 0.000000000000000000 ) ) ;
#3511 = ORIENTED_EDGE ( 'NONE', *, *, #3947, .F. ) ;
#3512 = COLOUR_RGB ( '',1.000000000000000000, 0.9490196078431372140, 0.9098039215686274384 ) ;
#3513 = CARTESIAN_POINT ( 'NONE',  ( 11.00000000000000355, -2.488243985854232676E-14, 13.99999999999999645 ) ) ;
#3514 = DIRECTION ( 'NONE',  ( -0.000000000000000000, -0.000000000000000000, 1.000000000000000000 ) ) ;
#3515 = ORIENTED_EDGE ( 'NONE', *, *, #2379, .T. ) ;
#3516 = DIRECTION ( 'NONE',  ( -1.000000000000000000, 1.156482317317871725E-16, 0.000000000000000000 ) ) ;
#3517 = CARTESIAN_POINT ( 'NONE',  ( 2.597146444261842824, -5.700021143261160717, 13.99999999999999645 ) ) ;
#3518 = VERTEX_POINT ( 'NONE', #5440 ) ;
#3519 = ORIENTED_EDGE ( 'NONE', *, *, #4176, .F. ) ;
#3520 = CARTESIAN_POINT ( 'NONE',  ( -3.231338468933152797, -7.147216519672495494, 14.00000000000000000 ) ) ;
#3521 = CARTESIAN_POINT ( 'NONE',  ( 6.460119401626724489, -2.924461030940388895, 1.999999999999998224 ) ) ;
#3522 = FACE_BOUND ( 'NONE', #2000, .T. ) ;
#3523 = CARTESIAN_POINT ( 'NONE',  ( 7.017208779832877497, -5.019401656905778886, 14.00000000000000000 ) ) ;
#3524 = ORIENTED_EDGE ( 'NONE', *, *, #1540, .T. ) ;
#3525 = CARTESIAN_POINT ( 'NONE',  ( -5.250997584835956467, 8.145342823910020513, 1.999999999999998224 ) ) ;
#3526 =( GEOMETRIC_REPRESENTATION_CONTEXT ( 3 ) GLOBAL_UNCERTAINTY_ASSIGNED_CONTEXT ( ( #4493 ) ) GLOBAL_UNIT_ASSIGNED_CONTEXT ( ( #5249, #4806, #4384 ) ) REPRESENTATION_CONTEXT ( 'NONE', 'WORKASPACE' ) );
#3527 = CARTESIAN_POINT ( 'NONE',  ( 17.55913978494622896, -14.85518798308249266, -8.000000000000000000 ) ) ;
#3528 = CARTESIAN_POINT ( 'NONE',  ( 2.321214644803172522, -6.838859567843808662, 13.99999999999999645 ) ) ;
#3529 = VECTOR ( 'NONE', #514, 1000.000000000000000 ) ;
#3530 = APPLICATION_PROTOCOL_DEFINITION ( 'draft international standard', 'automotive_design', 1998, #1512 ) ;
#3531 = CARTESIAN_POINT ( 'NONE',  ( 7.990059919442647818, -3.149571442993177595, 1.999999999999998224 ) ) ;
#3532 = CARTESIAN_POINT ( 'NONE',  ( 6.804422688527091978, 1.586354726853912434, 1.999999999999998224 ) ) ;
#3533 = AXIS2_PLACEMENT_3D ( 'NONE', #4735, #1178, #801 ) ;
#3534 = CARTESIAN_POINT ( 'NONE',  ( 17.74999999999999289, -15.01665741768121443, -4.000000000000000000 ) ) ;
#3535 = DIRECTION ( 'NONE',  ( -0.000000000000000000, -0.5000000000000002220, 0.8660254037844384856 ) ) ;
#3536 = VECTOR ( 'NONE', #3992, 1000.000000000000114 ) ;
#3537 = COLOUR_RGB ( '',0.8941176470588234615, 0.8941176470588234615, 0.8941176470588234615 ) ;
#3538 = CARTESIAN_POINT ( 'NONE',  ( 3.173694703385744997, 5.505084763670540227, 1.999999999999998224 ) ) ;
#3539 = LINE ( 'NONE', #1410, #4850 ) ;
#3540 = ORIENTED_EDGE ( 'NONE', *, *, #4575, .T. ) ;
#3541 = FACE_OUTER_BOUND ( 'NONE', #5315, .T. ) ;
#3542 = AXIS2_PLACEMENT_3D ( 'NONE', #3603, #5358, #4522 ) ;
#3543 = CARTESIAN_POINT ( 'NONE',  ( 10.40193138080327628, 3.529992181067589829, 13.99999999999999645 ) ) ;
#3544 = DIRECTION ( 'NONE',  ( 0.000000000000000000, 0.000000000000000000, -1.000000000000000000 ) ) ;
#3545 = CIRCLE ( 'NONE', #5664, 4.324969328314201888 ) ;
#3546 = FACE_OUTER_BOUND ( 'NONE', #4190, .T. ) ;
#3547 = ORIENTED_EDGE ( 'NONE', *, *, #1083, .T. ) ;
#3548 = ORIENTED_EDGE ( 'NONE', *, *, #3416, .F. ) ;
#3549 = CARTESIAN_POINT ( 'NONE',  ( -7.986673696634112751, -0.6581801297105769333, 14.00000000000000000 ) ) ;
#3550 = CARTESIAN_POINT ( 'NONE',  ( 3.471913601335177013, 7.039518430846525732, 1.999999999999998224 ) ) ;
#3551 = CIRCLE ( 'NONE', #1528, 25.00000000000000000 ) ;
#3552 = DIRECTION ( 'NONE',  ( -0.000000000000000000, 1.000000000000000000, -0.000000000000000000 ) ) ;
#3553 = CARTESIAN_POINT ( 'NONE',  ( -8.013356705133178437, 0.6503825268544297655, 14.00000000000000000 ) ) ;
#3554 = ORIENTED_EDGE ( 'NONE', *, *, #352, .F. ) ;
#3555 = EDGE_CURVE ( 'NONE', #1462, #2377, #608, .T. ) ;
#3556 = AXIS2_PLACEMENT_3D ( 'NONE', #3411, #3466, #5163 ) ;
#3557 = CARTESIAN_POINT ( 'NONE',  ( -7.945634105012028492, -6.745245841440164369, 1.999999999999998224 ) ) ;
#3558 = CARTESIAN_POINT ( 'NONE',  ( 5.500000000000001776, 0.000000000000000000, 14.00000000000000000 ) ) ;
#3559 = CARTESIAN_POINT ( 'NONE',  ( 6.824478893064963358, -1.828844244265460217, 13.99999999999999645 ) ) ;
#3560 = VECTOR ( 'NONE', #341, 1000.000000000000000 ) ;
#3561 = EDGE_CURVE ( 'NONE', #5130, #4336, #977, .T. ) ;
#3562 = APPLICATION_PROTOCOL_DEFINITION ( 'draft international standard', 'automotive_design', 1998, #1809 ) ;
#3563 = CARTESIAN_POINT ( 'NONE',  ( 7.379526280503348801, 5.862399640741291051, 1.999999999999998224 ) ) ;
#3564 = CARTESIAN_POINT ( 'NONE',  ( -6.465640026559585252, 4.020973141381892546, 1.999999999999998224 ) ) ;
#3565 = AXIS2_PLACEMENT_3D ( 'NONE', #1801, #2149, #3903 ) ;
#3566 = SURFACE_STYLE_FILL_AREA ( #1807 ) ;
#3567 = EDGE_CURVE ( 'NONE', #3442, #3843, #1153, .T. ) ;
#3568 = UNCERTAINTY_MEASURE_WITH_UNIT (LENGTH_MEASURE( 1.000000000000000082E-05 ), #3995, 'distance_accuracy_value', 'NONE');
#3569 = CARTESIAN_POINT ( 'NONE',  ( 22.00000000000000000, 0.000000000000000000, 4.000000000000001776 ) ) ;
#3570 = CARTESIAN_POINT ( 'NONE',  ( -1.336592501075286599, -5.709464570123371274, 1.999999999999998224 ) ) ;
#3571 = CARTESIAN_POINT ( 'NONE',  ( 5.326024957120312209, -1.813589758486610970, 1.999999999999998224 ) ) ;
#3572 = CARTESIAN_POINT ( 'NONE',  ( 1.300000000000000044, 1.082531754730548856, -0.6250000000000003331 ) ) ;
#3573 = ORIENTED_EDGE ( 'NONE', *, *, #2928, .T. ) ;
#3574 = CARTESIAN_POINT ( 'NONE',  ( -5.399999999999998579, 26.45448922205832787, 24.08672805191341482 ) ) ;
#3575 = CARTESIAN_POINT ( 'NONE',  ( 0.1774200004017887078, 10.78715707688374614, 13.99999999999999645 ) ) ;
#3576 = APPLICATION_CONTEXT ( 'automotive_design' ) ;
#3577 =( NAMED_UNIT ( * ) PLANE_ANGLE_UNIT ( ) SI_UNIT ( $, .RADIAN. ) );
#3578 = PLANE ( 'NONE',  #1796 ) ;
#3579 = ORIENTED_EDGE ( 'NONE', *, *, #3090, .F. ) ;
#3580 = EDGE_CURVE ( 'NONE', #3473, #261, #178, .T. ) ;
#3581 = CARTESIAN_POINT ( 'NONE',  ( 23.00000000000000000, 2.816687638038912352E-15, 8.000000000000000000 ) ) ;
#3582 = CARTESIAN_POINT ( 'NONE',  ( 4.853468040355885194, -8.397360160973688537, 14.00000000000000000 ) ) ;
#3583 = CARTESIAN_POINT ( 'NONE',  ( -3.989331152809321157, -6.191695749071041810, 1.999999999999998224 ) ) ;
#3584 = CARTESIAN_POINT ( 'NONE',  ( 8.453438707198472457, 0.9797652757261496870, 1.999999999999998224 ) ) ;
#3585 = CARTESIAN_POINT ( 'NONE',  ( 9.522148329495834673, -0.6196525284526704924, 14.00000000000000000 ) ) ;
#3586 = VERTEX_POINT ( 'NONE', #2417 ) ;
#3587 = CARTESIAN_POINT ( 'NONE',  ( 6.019515613300546519, 7.843576796802394391, 1.999999999999998224 ) ) ;
#3588 = DIRECTION ( 'NONE',  ( -0.000000000000000000, -0.000000000000000000, 1.000000000000000000 ) ) ;
#3589 = CARTESIAN_POINT ( 'NONE',  ( 7.761517335261691741, -2.213789340049631349, 13.99999999999999645 ) ) ;
#3590 = CARTESIAN_POINT ( 'NONE',  ( -2.721086536275892254, 7.222755814214462333, 13.99999999999999645 ) ) ;
#3591 = CARTESIAN_POINT ( 'NONE',  ( 6.591354251721933011, -5.587324598951576071, 1.999999999999998224 ) ) ;
#3592 = EDGE_CURVE ( 'NONE', #73, #5180, #4380, .T. ) ;
#3593 = CARTESIAN_POINT ( 'NONE',  ( -5.810612947751084612, -4.611264106266946605, 1.999999999999998224 ) ) ;
#3594 =( LENGTH_UNIT ( ) NAMED_UNIT ( * ) SI_UNIT ( .MILLI., .METRE. ) );
#3595 = CYLINDRICAL_SURFACE ( 'NONE', #2335, 23.00000000000000000 ) ;
#3596 = SURFACE_STYLE_USAGE ( .BOTH. , #2188 ) ;
#3597 = CARTESIAN_POINT ( 'NONE',  ( 1.300000000000000044, -0.7216878364870318308, -1.250000000000000000 ) ) ;
#3598 = CARTESIAN_POINT ( 'NONE',  ( 4.999999999999914735, 24.49489742783179835, -8.000000000000000000 ) ) ;
#3599 = DIRECTION ( 'NONE',  ( -0.2000000000000000111, 0.9797958971132711969, 0.000000000000000000 ) ) ;
#3600 = FILL_AREA_STYLE ('',( #952 ) ) ;
#3601 = CARTESIAN_POINT ( 'NONE',  ( 2.810994617404221962, -9.846529629020569274, 13.99999999999999645 ) ) ;
#3602 = CARTESIAN_POINT ( 'NONE',  ( 10.20000000000000107, 2.210487472460972205E-16, -1.610000000000000098 ) ) ;
#3603 = CARTESIAN_POINT ( 'NONE',  ( 0.000000000000000000, 0.000000000000000000, 8.000000000000000000 ) ) ;
#3604 = VERTEX_POINT ( 'NONE', #1123 ) ;
#3605 = ORIENTED_EDGE ( 'NONE', *, *, #4046, .T. ) ;
#3606 = COLOUR_RGB ( '',0.8941176470588234615, 0.8941176470588234615, 0.8941176470588234615 ) ;
#3607 = CARTESIAN_POINT ( 'NONE',  ( 5.710084532570044225, 7.448680193042861220, 14.00000000000000000 ) ) ;
#3608 = CARTESIAN_POINT ( 'NONE',  ( 6.804422688527091978, 1.586354726853912434, 1.999999999999998224 ) ) ;
#3609 = CARTESIAN_POINT ( 'NONE',  ( 6.591354251721933011, -5.587324598951576071, 1.999999999999998224 ) ) ;
#3610 = PRODUCT_DEFINITION_FORMATION_WITH_SPECIFIED_SOURCE ( 'ANY', '', #4680, .NOT_KNOWN. ) ;
#3611 = CARTESIAN_POINT ( 'NONE',  ( -7.966005157978615969, 4.422220743486623640, 14.00000000000000000 ) ) ;
#3612 = ORIENTED_EDGE ( 'NONE', *, *, #1530, .F. ) ;
#3613 = CARTESIAN_POINT ( 'NONE',  ( -0.7976699882155984245, 9.736979168371712845, 1.999999999999998224 ) ) ;
#3614 = FACE_OUTER_BOUND ( 'NONE', #1248, .T. ) ;
#3615 = CARTESIAN_POINT ( 'NONE',  ( 8.396466517618241809, 3.163083589105052607, 13.99999999999999645 ) ) ;
#3616 = CARTESIAN_POINT ( 'NONE',  ( -8.513020831365363250, 0.6954046021538080602, 13.99999999999999645 ) ) ;
#3617 = CARTESIAN_POINT ( 'NONE',  ( -5.637968025906140213, -2.116521738900702942, 14.00000000000000000 ) ) ;
#3618 = CARTESIAN_POINT ( 'NONE',  ( 7.344045208304290639, 5.086154276871864610, 1.999999999999998224 ) ) ;
#3619 = ADVANCED_FACE ( 'NONE', ( #4095 ), #1561, .F. ) ;
#3620 = CIRCLE ( 'NONE', #4906, 1.999999999999999112 ) ;
#3621 = DIRECTION ( 'NONE',  ( 0.06000000000000008105, -0.9981983770774224274, 0.000000000000000000 ) ) ;
#3622 = CARTESIAN_POINT ( 'NONE',  ( -2.283612537812033771, 5.775797914528922661, 1.999999999999998224 ) ) ;
#3623 = VERTEX_POINT ( 'NONE', #5064 ) ;
#3624 = CARTESIAN_POINT ( 'NONE',  ( 0.000000000000000000, 0.000000000000000000, -8.000000000000000000 ) ) ;
#3625 = CIRCLE ( 'NONE', #1420, 25.00000000000000000 ) ;
#3626 = CARTESIAN_POINT ( 'NONE',  ( 4.999999999999923617, 22.44994432064366308, 8.000000000000000000 ) ) ;
#3627 = CARTESIAN_POINT ( 'NONE',  ( -4.256527737016168267, -4.845957569453232416, 13.99999999999999645 ) ) ;
#3628 = VECTOR ( 'NONE', #5667, 1000.000000000000000 ) ;
#3629 = CARTESIAN_POINT ( 'NONE',  ( 22.99999999999999645, -8.485281374238580199, 4.000000000000000000 ) ) ;
#3630 = DIRECTION ( 'NONE',  ( 1.000000000000000000, 0.000000000000000000, 0.000000000000000000 ) ) ;
#3631 = LINE ( 'NONE', #4435, #2813 ) ;
#3632 = ORIENTED_EDGE ( 'NONE', *, *, #2172, .T. ) ;
#3633 = VECTOR ( 'NONE', #4718, 1000.000000000000000 ) ;
#3634 = ORIENTED_EDGE ( 'NONE', *, *, #3459, .F. ) ;
#3635 = CARTESIAN_POINT ( 'NONE',  ( -6.681386044268952773, 6.252046474378028407, 14.00000000000000000 ) ) ;
#3636 = CARTESIAN_POINT ( 'NONE',  ( 5.586635445632133212, -4.430858740432559451, 1.999999999999998224 ) ) ;
#3637 = ADVANCED_FACE ( 'NONE', ( #5470 ), #1526, .T. ) ;
#3638 = EDGE_CURVE ( 'NONE', #2009, #534, #3371, .T. ) ;
#3639 = CARTESIAN_POINT ( 'NONE',  ( -7.945923533235636604, 1.308497053349305439, 1.999999999999998224 ) ) ;
#3640 = CARTESIAN_POINT ( 'NONE',  ( -8.072272399573057200, -5.790267008922743486, 14.00000000000000000 ) ) ;
#3641 = ORIENTED_EDGE ( 'NONE', *, *, #5258, .F. ) ;
#3642 = CARTESIAN_POINT ( 'NONE',  ( 2.803319092186594030, 10.45862564946446760, 1.999999999999998224 ) ) ;
#3643 = CARTESIAN_POINT ( 'NONE',  ( -5.183646570197097958, -3.010418922386785212, 14.00000000000000000 ) ) ;
#3644 = CARTESIAN_POINT ( 'NONE',  ( 7.812003909081977504, 1.689803927524662797, 13.99999999999999645 ) ) ;
#3645 = VECTOR ( 'NONE', #1096, 1000.000000000000000 ) ;
#3646 = CARTESIAN_POINT ( 'NONE',  ( -2.067895747887561697, -9.596367745172036834, 1.999999999999998224 ) ) ;
#3647 = AXIS2_PLACEMENT_3D ( 'NONE', #4636, #5418, #205 ) ;
#3648 = ORIENTED_EDGE ( 'NONE', *, *, #1864, .F. ) ;
#3649 = CARTESIAN_POINT ( 'NONE',  ( 0.5432484998931219611, -8.249156888542632515, 1.999999999999998224 ) ) ;
#3650 = EDGE_CURVE ( 'NONE', #4295, #4159, #5117, .T. ) ;
#3651 = AXIS2_PLACEMENT_3D ( 'NONE', #712, #2401, #1077 ) ;
#3652 = DIRECTION ( 'NONE',  ( 1.000000000000000000, 0.000000000000000000, 0.000000000000000000 ) ) ;
#3653 =( NAMED_UNIT ( * ) PLANE_ANGLE_UNIT ( ) SI_UNIT ( $, .RADIAN. ) );
#3654 = CARTESIAN_POINT ( 'NONE',  ( -5.637968025906138436, -2.116521738900817073, 1.999999999999998224 ) ) ;
#3655 = EDGE_LOOP ( 'NONE', ( #2683, #1783, #711, #5573 ) ) ;
#3656 = AXIS2_PLACEMENT_3D ( 'NONE', #367, #4684, #744 ) ;
#3657 = CARTESIAN_POINT ( 'NONE',  ( 6.680730669075649608, 3.301097878975988387, 1.999999999999998224 ) ) ;
#3658 = DIRECTION ( 'NONE',  ( 1.000000000000000000, 0.000000000000000000, -0.000000000000000000 ) ) ;
#3659 = CARTESIAN_POINT ( 'NONE',  ( 0.000000000000000000, 0.000000000000000000, -58.22539674441618018 ) ) ;
#3660 =( NAMED_UNIT ( * ) SI_UNIT ( $, .STERADIAN. ) SOLID_ANGLE_UNIT ( ) );
#3661 = ADVANCED_FACE ( 'NONE', ( #2450 ), #3002, .T. ) ;
#3662 = CARTESIAN_POINT ( 'NONE',  ( 10.75001815606828970, 0.003012922916577078902, 14.00000000000000000 ) ) ;
#3663 = ORIENTED_EDGE ( 'NONE', *, *, #1203, .T. ) ;
#3664 = CARTESIAN_POINT ( 'NONE',  ( 23.48484848484848442, -8.570991287109677614, -8.000000000000000000 ) ) ;
#3665 = CARTESIAN_POINT ( 'NONE',  ( 6.721134410589271191, -6.938257756002876420, 14.00000000000000000 ) ) ;
#3666 = CARTESIAN_POINT ( 'NONE',  ( -5.210352092881994857, -6.569156856910357334, 1.999999999999998224 ) ) ;
#3667 = CARTESIAN_POINT ( 'NONE',  ( -7.652305818843809782, 2.590529227167489790, 1.999999999999998224 ) ) ;
#3668 = CARTESIAN_POINT ( 'NONE',  ( 8.172274133038307298, -5.076547540501183065, 14.00000000000000000 ) ) ;
#3669 = ORIENTED_EDGE ( 'NONE', *, *, #1191, .T. ) ;
#3670 = DIRECTION ( 'NONE',  ( 0.000000000000000000, 0.000000000000000000, 1.000000000000000000 ) ) ;
#3671 = CARTESIAN_POINT ( 'NONE',  ( 3.173694703385745886, 5.505084763670784476, 14.00000000000000000 ) ) ;
#3672 = CARTESIAN_POINT ( 'NONE',  ( 9.020117466465418232, 0.2947087185667972564, 13.99999999999999645 ) ) ;
#3673 = CARTESIAN_POINT ( 'NONE',  ( 1.837295235934470305, 10.14794156482770049, 1.999999999999998224 ) ) ;
#3674 = EDGE_LOOP ( 'NONE', ( #2678, #1432, #5089, #5071, #356, #4537 ) ) ;
#3675 = CARTESIAN_POINT ( 'NONE',  ( 4.043470907200509501, 7.877814422643418801, 1.999999999999998224 ) ) ;
#3676 = DIRECTION ( 'NONE',  ( -1.000000000000000000, -0.000000000000000000, -0.000000000000000000 ) ) ;
#3677 = CARTESIAN_POINT ( 'NONE',  ( -6.065725208710914806, -3.376743199310592747, 1.999999999999998224 ) ) ;
#3678 = EDGE_CURVE ( 'NONE', #2953, #4241, #3545, .T. ) ;
#3679 = EDGE_LOOP ( 'NONE', ( #4753, #4791 ) ) ;
#3680 = CARTESIAN_POINT ( 'NONE',  ( 2.672042568001582019, -6.151894458593051063, 1.999999999999998224 ) ) ;
#3681 = LINE ( 'NONE', #569, #3386 ) ;
#3682 = DIRECTION ( 'NONE',  ( -1.000000000000000000, -0.000000000000000000, -0.000000000000000000 ) ) ;
#3683 = DIRECTION ( 'NONE',  ( -0.000000000000000000, -0.000000000000000000, -1.000000000000000000 ) ) ;
#3684 = CARTESIAN_POINT ( 'NONE',  ( 0.000000000000000000, 0.000000000000000000, 14.00000000000000000 ) ) ;
#3685 = DIRECTION ( 'NONE',  ( 1.000000000000000000, 0.000000000000000000, 0.000000000000000000 ) ) ;
#3686 = ORIENTED_EDGE ( 'NONE', *, *, #257, .F. ) ;
#3687 = LINE ( 'NONE', #5442, #798 ) ;
#3688 = CARTESIAN_POINT ( 'NONE',  ( 6.863489721961782308, 6.439594285166703180, 14.00000000000000000 ) ) ;
#3689 = CARTESIAN_POINT ( 'NONE',  ( 8.640499015841685448, 2.466831329604985079, 1.999999999999998224 ) ) ;
#3690 = CARTESIAN_POINT ( 'NONE',  ( -3.109042548464319378, -8.271822080922653697, 1.999999999999998224 ) ) ;
#3691 = CARTESIAN_POINT ( 'NONE',  ( -7.588772809867895930, -4.728083520431684228, 14.00000000000000000 ) ) ;
#3692 = DIRECTION ( 'NONE',  ( 1.000000000000000000, 0.000000000000000000, 0.000000000000000000 ) ) ;
#3693 = VERTEX_POINT ( 'NONE', #1957 ) ;
#3694 = DIRECTION ( 'NONE',  ( 0.000000000000000000, 0.000000000000000000, 1.000000000000000000 ) ) ;
#3695 = CARTESIAN_POINT ( 'NONE',  ( 4.500000000000000888, 0.000000000000000000, 0.000000000000000000 ) ) ;
#3696 = CARTESIAN_POINT ( 'NONE',  ( -3.798941939731700579, -9.621416145859109648, 13.99999999999999645 ) ) ;
#3697 = CARTESIAN_POINT ( 'NONE',  ( -9.445900372709948201, 3.550092993115765871, 1.999999999999998224 ) ) ;
#3698 = EDGE_LOOP ( 'NONE', ( #3902, #4264, #4387, #4835, #2362 ) ) ;
#3699 = CARTESIAN_POINT ( 'NONE',  ( -8.513020831365363250, 0.6954046021538080602, 1.999999999999998224 ) ) ;
#3700 = CARTESIAN_POINT ( 'NONE',  ( 0.000000000000000000, 0.000000000000000000, -8.000000000000000000 ) ) ;
#3701 =( NAMED_UNIT ( * ) SI_UNIT ( $, .STERADIAN. ) SOLID_ANGLE_UNIT ( ) );
#3702 = CARTESIAN_POINT ( 'NONE',  ( 0.9466184546083533657, 7.233353930637701268, 1.999999999999998224 ) ) ;
#3703 = ORIENTED_EDGE ( 'NONE', *, *, #3638, .F. ) ;
#3704 = CARTESIAN_POINT ( 'NONE',  ( 3.621982275015807051, -5.614208739972523787, 1.999999999999998224 ) ) ;
#3705 = DIRECTION ( 'NONE',  ( -3.540989467475305966E-16, -1.000000000000000000, 0.000000000000000000 ) ) ;
#3706 = FILL_AREA_STYLE_COLOUR ( '', #433 ) ;
#3707 = VECTOR ( 'NONE', #1839, 1000.000000000000000 ) ;
#3708 = CARTESIAN_POINT ( 'NONE',  ( 0.000000000000000000, 0.000000000000000000, 0.000000000000000000 ) ) ;
#3709 = CARTESIAN_POINT ( 'NONE',  ( 0.000000000000000000, 0.000000000000000000, 5.000000000000000000 ) ) ;
#3710 = CARTESIAN_POINT ( 'NONE',  ( 1.380000000000002558, 22.95856267278071527, 1.371299631966804711 ) ) ;
#3711 = EDGE_LOOP ( 'NONE', ( #2307, #4927, #2108, #2551 ) ) ;
#3712 = CARTESIAN_POINT ( 'NONE',  ( 1.300000000000000044, -0.7216878364870318308, 1.249999999999999778 ) ) ;
#3713 = DIRECTION ( 'NONE',  ( -0.000000000000000000, -0.000000000000000000, -1.000000000000000000 ) ) ;
#3714 = CARTESIAN_POINT ( 'NONE',  ( 5.347643153870339283, -7.463670412152253242, 1.999999999999998224 ) ) ;
#3715 = AXIS2_PLACEMENT_3D ( 'NONE', #2321, #3246, #657 ) ;
#3716 = CARTESIAN_POINT ( 'NONE',  ( 1.649120185255091187, 7.633850905136058351, 13.99999999999999645 ) ) ;
#3717 = EDGE_CURVE ( 'NONE', #5180, #73, #4286, .T. ) ;
#3718 = CARTESIAN_POINT ( 'NONE',  ( -6.708753103182418798, 7.642576097240645794, 1.999999999999998224 ) ) ;
#3719 = DIRECTION ( 'NONE',  ( -1.000000000000000000, 0.000000000000000000, 0.000000000000000000 ) ) ;
#3721 = VERTEX_POINT ( 'NONE', #3058 ) ;
#3720 = VECTOR ( 'NONE', #974, 1000.000000000000000 ) ;
#3722 = CARTESIAN_POINT ( 'NONE',  ( 1.820000000000000062, -3.800000000000000266, -4.653657836759940757E-16 ) ) ;
#3723 = VERTEX_POINT ( 'NONE', #3916 ) ;
#3724 = LINE ( 'NONE', #1940, #2357 ) ;
#3725 = CARTESIAN_POINT ( 'NONE',  ( -6.041022033915573353, 3.753782041847178341, 14.00000000000000000 ) ) ;
#3726 = CARTESIAN_POINT ( 'NONE',  ( -3.867583043141954224, 8.914321633329153727, 13.99999999999999645 ) ) ;
#3727 = AXIS2_PLACEMENT_3D ( 'NONE', #2019, #3773, #4294 ) ;
#3728 = CARTESIAN_POINT ( 'NONE',  ( -9.926332099420363875, -1.311590842189569894, 1.999999999999998224 ) ) ;
#3729 = ORIENTED_EDGE ( 'NONE', *, *, #3915, .T. ) ;
#3730 = AXIS2_PLACEMENT_3D ( 'NONE', #3229, #148, #4180 ) ;
#3731 = CARTESIAN_POINT ( 'NONE',  ( -9.533152408061617678, 0.1566715252477025866, 1.999999999999998224 ) ) ;
#3732 = CARTESIAN_POINT ( 'NONE',  ( -1.380000000000000115, 22.95856267278071527, 12.00000000000000000 ) ) ;
#3733 = CLOSED_SHELL ( 'NONE', ( #2008, #4770, #3048, #962, #5652, #5302, #88, #4085, #2235, #2832, #3173, #3637, #5081, #910, #4338, #124, #853, #1705, #2616, #383, #2061, #850, #2618, #3931, #4314, #2790, #4875 ) ) ;
#3734 = CIRCLE ( 'NONE', #5023, 12.50000000000000000 ) ;
#3735 = CARTESIAN_POINT ( 'NONE',  ( -4.089163901200156381, 5.898691170885093982, 1.999999999999998224 ) ) ;
#3736 = VERTEX_POINT ( 'NONE', #1698 ) ;
#3737 = CARTESIAN_POINT ( 'NONE',  ( 1.103627080440590102, -6.655442145117440589, 1.999999999999998224 ) ) ;
#3738 = DIRECTION ( 'NONE',  ( 0.000000000000000000, 0.000000000000000000, 1.000000000000000000 ) ) ;
#3739 = EDGE_CURVE ( 'NONE', #1333, #5441, #2561, .T. ) ;
#3740 = CIRCLE ( 'NONE', #4292, 25.00000000000000000 ) ;
#3741 = DIRECTION ( 'NONE',  ( 1.000000000000000000, 0.000000000000000000, 0.000000000000000000 ) ) ;
#3742 = CARTESIAN_POINT ( 'NONE',  ( 2.021687836487040535, 0.000000000000000000, 2.168404344971008868E-16 ) ) ;
#3743 = AXIS2_PLACEMENT_3D ( 'NONE', #4378, #3143, #3599 ) ;
#3744 = DIRECTION ( 'NONE',  ( 0.000000000000000000, 0.000000000000000000, 1.000000000000000000 ) ) ;
#3745 = EDGE_CURVE ( 'NONE', #1983, #5180, #2530, .T. ) ;
#3746 = EDGE_LOOP ( 'NONE', ( #1228, #2974, #2372, #3663 ) ) ;
#3747 = CARTESIAN_POINT ( 'NONE',  ( -2.199999999999999289, 2.694222958124176020E-16, -3.100000000000000533 ) ) ;
#3748 = CARTESIAN_POINT ( 'NONE',  ( -0.6809175113353355124, 10.25113960786383949, 14.00000000000000000 ) ) ;
#3749 = CARTESIAN_POINT ( 'NONE',  ( 1.999247522871089311, 8.586038698136235325, 1.999999999999998224 ) ) ;
#3750 = CARTESIAN_POINT ( 'NONE',  ( -7.519441789400338472, 0.4931591957933217363, 13.99999999999999645 ) ) ;
#3751 = CARTESIAN_POINT ( 'NONE',  ( 15.00000000000000000, 1.836970198721029589E-15, 12.00000000000000000 ) ) ;
#3752 = EDGE_CURVE ( 'NONE', #5536, #4755, #1300, .T. ) ;
#3753 = ORIENTED_EDGE ( 'NONE', *, *, #1203, .F. ) ;
#3754 = DIRECTION ( 'NONE',  ( -1.000000000000000000, 0.000000000000000000, 0.000000000000000000 ) ) ;
#3755 = ORIENTED_EDGE ( 'NONE', *, *, #3678, .T. ) ;
#3756 = DIRECTION ( 'NONE',  ( -0.000000000000000000, -0.5000000000000002220, 0.8660254037844384856 ) ) ;
#3757 = CARTESIAN_POINT ( 'NONE',  ( 6.034497645749724803, 4.327592090611794617, 14.00000000000000000 ) ) ;
#3758 = CARTESIAN_POINT ( 'NONE',  ( 9.650319724629330409, 2.588775111615905011, 13.99999999999999645 ) ) ;
#3759 = CARTESIAN_POINT ( 'NONE',  ( -6.734745854536168252, 2.161492950162117399, 14.00000000000000000 ) ) ;
#3760 = APPLICATION_CONTEXT ( 'automotive_design' ) ;
#3761 = EDGE_LOOP ( 'NONE', ( #2206, #3036, #2863, #2178 ) ) ;
#3762 = CARTESIAN_POINT ( 'NONE',  ( -5.893815055328603947, 7.676334994785346311, 1.999999999999998224 ) ) ;
#3763 = PRODUCT_DEFINITION_SHAPE ( 'NONE', 'NONE',  #4780 ) ;
#3764 = CARTESIAN_POINT ( 'NONE',  ( 0.000000000000000000, 0.000000000000000000, -8.000000000000000000 ) ) ;
#3765 = PRODUCT_RELATED_PRODUCT_CATEGORY ( 'part', '', ( #5046 ) ) ;
#3766 = CARTESIAN_POINT ( 'NONE',  ( 6.034497645749723027, 4.327592090611793729, 1.999999999999998224 ) ) ;
#3767 = ORIENTED_EDGE ( 'NONE', *, *, #4164, .F. ) ;
#3768 = CARTESIAN_POINT ( 'NONE',  ( 4.776808680784692562, 5.634249062854761014, 1.999999999999998224 ) ) ;
#3769 = CARTESIAN_POINT ( 'NONE',  ( 0.000000000000000000, 0.000000000000000000, 0.000000000000000000 ) ) ;
#3770 = CARTESIAN_POINT ( 'NONE',  ( -3.845892476879857469, 6.661954734853424043, 13.99999999999999645 ) ) ;
#3771 = UNCERTAINTY_MEASURE_WITH_UNIT (LENGTH_MEASURE( 1.000000000000000082E-05 ), #1268, 'distance_accuracy_value', 'NONE');
#3772 = CARTESIAN_POINT ( 'NONE',  ( 10.50003631213658117, 0.006025845833179007717, 14.00000000000000000 ) ) ;
#3773 = DIRECTION ( 'NONE',  ( -0.000000000000000000, -0.000000000000000000, -1.000000000000000000 ) ) ;
#3774 = ORIENTED_EDGE ( 'NONE', *, *, #2522, .F. ) ;
#3775 = DIRECTION ( 'NONE',  ( -0.000000000000000000, -0.000000000000000000, 1.000000000000000000 ) ) ;
#3776 = CARTESIAN_POINT ( 'NONE',  ( 0.000000000000000000, 0.000000000000000000, -3.100000000000000533 ) ) ;
#3777 = CARTESIAN_POINT ( 'NONE',  ( -8.486979168634645632, -0.6954046021538184963, 1.999999999999998224 ) ) ;
#3778 = CARTESIAN_POINT ( 'NONE',  ( 7.937472058415492526, 1.044590838406009858, 13.99999999999999645 ) ) ;
#3779 = ADVANCED_FACE ( 'NONE', ( #2074 ), #1346, .F. ) ;
#3780 = CARTESIAN_POINT ( 'NONE',  ( -5.391417556047953141, 8.653185861734563389, 14.00000000000000000 ) ) ;
#3781 = ORIENTED_EDGE ( 'NONE', *, *, #4072, .F. ) ;
#3782 = PLANE ( 'NONE',  #2255 ) ;
#3783 = EDGE_LOOP ( 'NONE', ( #333, #2666, #3230, #3060 ) ) ;
#3784 = CARTESIAN_POINT ( 'NONE',  ( -5.000000000000085265, 24.49489742783176638, 5.000000000000000000 ) ) ;
#3785 = CARTESIAN_POINT ( 'NONE',  ( -0.2403693791185868289, 7.265099133626555350, 14.00000000000000000 ) ) ;
#3786 = CARTESIAN_POINT ( 'NONE',  ( 9.077580196901687160, 4.112174628513754371, 13.99999999999999645 ) ) ;
#3787 = EDGE_CURVE ( 'NONE', #2713, #3462, #1623, .T. ) ;
#3788 = CARTESIAN_POINT ( 'NONE',  ( 3.247347166530789586, 6.590896817052466439, 14.00000000000000000 ) ) ;
#3789 = EDGE_LOOP ( 'NONE', ( #5226, #2050, #254, #5391 ) ) ;
#3790 = CARTESIAN_POINT ( 'NONE',  ( -6.726831604608804582, -7.927219868180728213, 1.999999999999998224 ) ) ;
#3791 = COLOUR_RGB ( '',0.8941176470588234615, 0.8941176470588234615, 0.8941176470588234615 ) ;
#3792 = CYLINDRICAL_SURFACE ( 'NONE', #3812, 0.2500000000000002220 ) ;
#3793 = CARTESIAN_POINT ( 'NONE',  ( 5.499810765991186123, -5.314180015047517358, 1.999999999999998224 ) ) ;
#3794 = FACE_OUTER_BOUND ( 'NONE', #2467, .T. ) ;
#3795 = CARTESIAN_POINT ( 'NONE',  ( -5.432680616552289621, 3.899654942172362748, 14.00000000000093792 ) ) ;
#3796 = EDGE_CURVE ( 'NONE', #1333, #3623, #606, .T. ) ;
#3797 =( LENGTH_UNIT ( ) NAMED_UNIT ( * ) SI_UNIT ( .MILLI., .METRE. ) );
#3798 = DIRECTION ( 'NONE',  ( -0.000000000000000000, -0.000000000000000000, 1.000000000000000000 ) ) ;
#3799 = FACE_OUTER_BOUND ( 'NONE', #4366, .T. ) ;
#3800 = ORIENTED_EDGE ( 'NONE', *, *, #5126, .T. ) ;
#3801 = CARTESIAN_POINT ( 'NONE',  ( 23.24999999999999645, -8.485281374238580199, 8.000000000000000000 ) ) ;
#3802 = DIRECTION ( 'NONE',  ( -1.000000000000000000, 0.000000000000000000, 0.000000000000000000 ) ) ;
#3803 = CARTESIAN_POINT ( 'NONE',  ( -7.080399483669990168, -6.208478756603781790, 1.999999999999998224 ) ) ;
#3804 = CIRCLE ( 'NONE', #309, 1.899999999999999689 ) ;
#3805 = CARTESIAN_POINT ( 'NONE',  ( 1.954797901281673633, -9.037865403626287986, 13.99999999999999645 ) ) ;
#3806 = EDGE_CURVE ( 'NONE', #5658, #3984, #4233, .T. ) ;
#3807 = CARTESIAN_POINT ( 'NONE',  ( -2.331745755519268215, 9.978964459600446091, 14.00000000000000000 ) ) ;
#3808 = ORIENTED_EDGE ( 'NONE', *, *, #3464, .T. ) ;
#3809 = CARTESIAN_POINT ( 'NONE',  ( 0.000000000000000000, 0.000000000000000000, 12.00000000000000000 ) ) ;
#3810 = ORIENTED_EDGE ( 'NONE', *, *, #1368, .F. ) ;
#3811 = DIRECTION ( 'NONE',  ( 0.000000000000000000, -1.224646799147353207E-16, 1.000000000000000000 ) ) ;
#3812 = AXIS2_PLACEMENT_3D ( 'NONE', #1979, #3365, #3307 ) ;
#3813 = CARTESIAN_POINT ( 'NONE',  ( 1.760389272475214373, -7.536528230137969686, 14.00000000000000000 ) ) ;
#3814 = EDGE_CURVE ( 'NONE', #92, #1194, #3481, .T. ) ;
#3815 = CARTESIAN_POINT ( 'NONE',  ( 7.631804465920718705, -6.689046765414282447, 13.99999999999999645 ) ) ;
#3816 = COLOUR_RGB ( '',0.8941176470588234615, 0.8941176470588234615, 0.8941176470588234615 ) ;
#3817 = VECTOR ( 'NONE', #3314, 1000.000000000000000 ) ;
#3818 = CARTESIAN_POINT ( 'NONE',  ( 5.772253124442537242, -3.205917188173946997, 14.00000000000000000 ) ) ;
#3819 = ORIENTED_EDGE ( 'NONE', *, *, #1553, .T. ) ;
#3820 = CARTESIAN_POINT ( 'NONE',  ( -7.044187934146015628, 6.598551529631267343, 1.999999999999998224 ) ) ;
#3821 = DIRECTION ( 'NONE',  ( -1.000000000000000000, 0.000000000000000000, 0.000000000000000000 ) ) ;
#3822 = SURFACE_STYLE_USAGE ( .BOTH. , #4625 ) ;
#3823 = CARTESIAN_POINT ( 'NONE',  ( -7.986673696634112751, -0.6581801297105769333, 1.999999999999998224 ) ) ;
#3824 = VECTOR ( 'NONE', #346, 1000.000000000000000 ) ;
#3825 = ADVANCED_FACE ( 'NONE', ( #3832 ), #5244, .T. ) ;
#3826 = DIRECTION ( 'NONE',  ( -0.000000000000000000, -0.000000000000000000, 1.000000000000000000 ) ) ;
#3827 = CARTESIAN_POINT ( 'NONE',  ( -7.364573508975984062, 1.714675912027187943, 13.99999999999999645 ) ) ;
#3828 = AXIS2_PLACEMENT_3D ( 'NONE', #1532, #1037, #151 ) ;
#3829 =( NAMED_UNIT ( * ) PLANE_ANGLE_UNIT ( ) SI_UNIT ( $, .RADIAN. ) );
#3830 = CARTESIAN_POINT ( 'NONE',  ( 4.853468040356245794, -8.397360160974407961, 1.999999999999998224 ) ) ;
#3831 = CIRCLE ( 'NONE', #4563, 25.00000000000000000 ) ;
#3832 = FACE_OUTER_BOUND ( 'NONE', #3952, .T. ) ;
#3833 = DIRECTION ( 'NONE',  ( -1.000000000000000000, 0.000000000000000000, 0.000000000000000000 ) ) ;
#3834 = ORIENTED_EDGE ( 'NONE', *, *, #1274, .T. ) ;
#3835 = DIRECTION ( 'NONE',  ( 1.000000000000000000, 0.000000000000000000, 0.000000000000000000 ) ) ;
#3836 = DIRECTION ( 'NONE',  ( -1.445602896647339163E-16, -0.000000000000000000, -1.000000000000000000 ) ) ;
#3837 = VECTOR ( 'NONE', #3705, 1000.000000000000000 ) ;
#3838 = CARTESIAN_POINT ( 'NONE',  ( -8.411612136543094920, -4.319922787977579226, 13.99999999999999645 ) ) ;
#3839 = PRODUCT_DEFINITION ( 'UNKNOWN', '', #4982, #3438 ) ;
#3840 = DIRECTION ( 'NONE',  ( -0.000000000000000000, -0.000000000000000000, 1.000000000000000000 ) ) ;
#3841 = VERTEX_POINT ( 'NONE', #3885 ) ;
#3842 = FACE_OUTER_BOUND ( 'NONE', #3345, .T. ) ;
#3843 = VERTEX_POINT ( 'NONE', #2160 ) ;
#3844 = AXIS2_PLACEMENT_3D ( 'NONE', #5411, #2298, #1090 ) ;
#3845 = DIRECTION ( 'NONE',  ( -0.000000000000000000, -0.000000000000000000, 1.000000000000000000 ) ) ;
#3846 = CARTESIAN_POINT ( 'NONE',  ( -6.742266116715659230, -1.811900715328871092, 14.00000000000000000 ) ) ;
#3847 = CARTESIAN_POINT ( 'NONE',  ( -4.256527737015712631, -4.845957569453684499, 1.999999999999998224 ) ) ;
#3848 = CARTESIAN_POINT ( 'NONE',  ( -6.334648143026945455, -2.872559841354017429, 14.00000000000000000 ) ) ;
#3849 = VERTEX_POINT ( 'NONE', #284 ) ;
#3850 = CARTESIAN_POINT ( 'NONE',  ( 8.993528569561179964, -4.616306094804414784, 1.999999999999998224 ) ) ;
#3851 = EDGE_CURVE ( 'NONE', #2920, #5392, #1731, .T. ) ;
#3852 = CARTESIAN_POINT ( 'NONE',  ( 2.200000000000000622, 0.000000000000000000, 2.199999999999999289 ) ) ;
#3853 = CARTESIAN_POINT ( 'NONE',  ( 3.247347166530788698, 6.590896817052186663, 1.999999999999998224 ) ) ;
#3854 = CARTESIAN_POINT ( 'NONE',  ( 2.597146444261841491, -5.700021143261159828, 1.999999999999998224 ) ) ;
#3855 = CARTESIAN_POINT ( 'NONE',  ( -0.8890388043606451962, 7.706404363472290520, 13.99999999999999645 ) ) ;
#3856 = ADVANCED_FACE ( 'NONE', ( #1185 ), #4745, .F. ) ;
#3857 = CARTESIAN_POINT ( 'NONE',  ( -9.692812185270616610, 2.758747493781260829, 1.999999999999998224 ) ) ;
#3858 = CARTESIAN_POINT ( 'NONE',  ( -1.380000000000002558, 21.95856267278071527, 15.94994774640597512 ) ) ;
#3859 = CARTESIAN_POINT ( 'NONE',  ( 0.000000000000000000, 0.000000000000000000, 8.000000000000000000 ) ) ;
#3860 = ORIENTED_EDGE ( 'NONE', *, *, #559, .T. ) ;
#3861 = DIRECTION ( 'NONE',  ( -1.000000000000000000, 0.000000000000000000, 0.000000000000000000 ) ) ;
#3862 = CARTESIAN_POINT ( 'NONE',  ( 23.00000000000000000, -8.144275775193202933E-15, 4.000000000000000000 ) ) ;
#3863 = CARTESIAN_POINT ( 'NONE',  ( 5.933674912743042817, -6.989438080420771193, 13.99999999999999645 ) ) ;
#3864 = CARTESIAN_POINT ( 'NONE',  ( 21.75000000000000000, 2.891205793294679929E-17, 12.00000000000000000 ) ) ;
#3865 = ORIENTED_EDGE ( 'NONE', *, *, #3555, .T. ) ;
#3866 = CYLINDRICAL_SURFACE ( 'NONE', #601, 1.999999999999999112 ) ;
#3867 = ORIENTED_EDGE ( 'NONE', *, *, #3806, .F. ) ;
#3868 = DIRECTION ( 'NONE',  ( -1.000000000000000000, -0.000000000000000000, -0.000000000000000000 ) ) ;
#3869 = CARTESIAN_POINT ( 'NONE',  ( 3.208073253695060245, -8.107602109809697311, 14.00000000000000000 ) ) ;
#3870 = CARTESIAN_POINT ( 'NONE',  ( -5.651290410005071152, 9.082320918485368821, 13.99999999999999645 ) ) ;
#3871 =( REPRESENTATION_RELATIONSHIP ('NONE','NONE', #4854, #1911 ) REPRESENTATION_RELATIONSHIP_WITH_TRANSFORMATION ( #507 )SHAPE_REPRESENTATION_RELATIONSHIP( ) );
#3872 = CARTESIAN_POINT ( 'NONE',  ( 0.000000000000000000, 0.000000000000000000, 0.000000000000000000 ) ) ;
#3873 = CARTESIAN_POINT ( 'NONE',  ( -5.416162817796315920, -4.301262981183149314, 14.00000000000000000 ) ) ;
#3874 = EDGE_LOOP ( 'NONE', ( #5360, #1627 ) ) ;
#3875 = CARTESIAN_POINT ( 'NONE',  ( 2.803319092186594030, 10.45862564946446760, 1.999999999999998224 ) ) ;
#3876 = CARTESIAN_POINT ( 'NONE',  ( 2.869471237997715640, -6.613103333303074649, 13.99999999999999645 ) ) ;
#3877 =( NAMED_UNIT ( * ) SI_UNIT ( $, .STERADIAN. ) SOLID_ANGLE_UNIT ( ) );
#3878 = CARTESIAN_POINT ( 'NONE',  ( 6.268835244667307904, -4.335177162149147279, 1.999999999999998224 ) ) ;
#3879 = DIRECTION ( 'NONE',  ( -1.000000000000000000, -0.000000000000000000, -0.000000000000000000 ) ) ;
#3880 = CARTESIAN_POINT ( 'NONE',  ( -6.505530684480628878, -3.618119970335913038, 13.99999999999999645 ) ) ;
#3881 = EDGE_CURVE ( 'NONE', #1950, #2855, #1063, .T. ) ;
#3882 =( GEOMETRIC_REPRESENTATION_CONTEXT ( 3 ) GLOBAL_UNCERTAINTY_ASSIGNED_CONTEXT ( ( #2238 ) ) GLOBAL_UNIT_ASSIGNED_CONTEXT ( ( #397, #5349, #2701 ) ) REPRESENTATION_CONTEXT ( 'NONE', 'WORKASPACE' ) );
#3883 =( NAMED_UNIT ( * ) SI_UNIT ( $, .STERADIAN. ) SOLID_ANGLE_UNIT ( ) );
#3884 = CARTESIAN_POINT ( 'NONE',  ( 2.667884741302309237, 9.975564253400264647, 1.999999999999998224 ) ) ;
#3885 = CARTESIAN_POINT ( 'NONE',  ( 1.820000000000000062, 4.653657836759941744E-16, -3.799999999999999378 ) ) ;
#3886 = DIRECTION ( 'NONE',  ( 0.000000000000000000, 0.000000000000000000, 1.000000000000000000 ) ) ;
#3887 = VERTEX_POINT ( 'NONE', #3374 ) ;
#3888 = CARTESIAN_POINT ( 'NONE',  ( 0.000000000000000000, 0.000000000000000000, -8.000000000000000000 ) ) ;
#3889 = CARTESIAN_POINT ( 'NONE',  ( 1.300000000000000044, 1.443375672974065216, 7.017607234860990640E-28 ) ) ;
#3890 = CARTESIAN_POINT ( 'NONE',  ( 1.598519525623709692, 9.677660462521252782, 13.99999999999999645 ) ) ;
#3891 = DIRECTION ( 'NONE',  ( 0.000000000000000000, 0.4999999999999999445, 0.8660254037844387076 ) ) ;
#3892 = ORIENTED_EDGE ( 'NONE', *, *, #500, .T. ) ;
#3893 = CARTESIAN_POINT ( 'NONE',  ( 23.24999999999999645, -8.485281374238580199, -8.000000000000000000 ) ) ;
#3894 = ORIENTED_EDGE ( 'NONE', *, *, #1780, .T. ) ;
#3895 = LINE ( 'NONE', #1628, #3016 ) ;
#3896 = CARTESIAN_POINT ( 'NONE',  ( -3.987536574861253236, 7.161134007378101352, 14.00000000000000000 ) ) ;
#3897 = CARTESIAN_POINT ( 'NONE',  ( -10.53467355220997526, 0.3418899515811328338, 13.99999999999999645 ) ) ;
#3898 = UNCERTAINTY_MEASURE_WITH_UNIT (LENGTH_MEASURE( 1.000000000000000082E-05 ), #1554, 'distance_accuracy_value', 'NONE');
#3899 = PLANE ( 'NONE',  #5459 ) ;
#3900 = CARTESIAN_POINT ( 'NONE',  ( -7.986673696634112751, -0.6581801297105769333, 14.00000000000000000 ) ) ;
#3901 = CIRCLE ( 'NONE', #4081, 23.00000000000000000 ) ;
#3902 = ORIENTED_EDGE ( 'NONE', *, *, #5588, .F. ) ;
#3903 = DIRECTION ( 'NONE',  ( -1.000000000000000000, 0.000000000000000000, 0.000000000000000000 ) ) ;
#3904 = AXIS2_PLACEMENT_3D ( 'NONE', #2872, #4252, #4624 ) ;
#3905 = CARTESIAN_POINT ( 'NONE',  ( 4.243312049792015372, -4.537448458213933833, 13.99999999999999645 ) ) ;
#3906 = CARTESIAN_POINT ( 'NONE',  ( 3.857245400775495714, -7.804869966781508239, 1.999999999999998224 ) ) ;
#3907 = PRODUCT_DEFINITION ( 'UNKNOWN', '', #2319, #2575 ) ;
#3908 = VECTOR ( 'NONE', #3111, 1000.000000000000000 ) ;
#3909 = ADVANCED_FACE ( 'NONE', ( #370, #5637 ), #3452, .F. ) ;
#3910 = CARTESIAN_POINT ( 'NONE',  ( 8.027649061863494140, -0.2602747315786821392, 1.999999999999998224 ) ) ;
#3911 = CARTESIAN_POINT ( 'NONE',  ( 4.326322805050086373, -6.952463250691143237, 13.99999999999999645 ) ) ;
#3912 = CARTESIAN_POINT ( 'NONE',  ( 0.000000000000000000, 0.000000000000000000, 24.08672805191341482 ) ) ;
#3913 = AXIS2_PLACEMENT_3D ( 'NONE', #2169, #3433, #5648 ) ;
#3914 = DIRECTION ( 'NONE',  ( 0.000000000000000000, 0.000000000000000000, 1.000000000000000000 ) ) ;
#3915 = EDGE_CURVE ( 'NONE', #1283, #36, #1271, .T. ) ;
#3916 = CARTESIAN_POINT ( 'NONE',  ( 1.300000000000000044, 0.7216878364870328300, -1.250000000000000000 ) ) ;
#3917 = CARTESIAN_POINT ( 'NONE',  ( 0.000000000000000000, 0.000000000000000000, 0.000000000000000000 ) ) ;
#3918 = VERTEX_POINT ( 'NONE', #3030 ) ;
#3919 = AXIS2_PLACEMENT_3D ( 'NONE', #2936, #4688, #749 ) ;
#3920 = CIRCLE ( 'NONE', #5643, 2.000000000000000000 ) ;
#3921 = CARTESIAN_POINT ( 'NONE',  ( 8.396466517618241809, 3.163083589105052607, 13.99999999999999645 ) ) ;
#3922 = MECHANICAL_DESIGN_GEOMETRIC_PRESENTATION_REPRESENTATION (  '', ( #4931 ), #3373 ) ;
#3923 = PRESENTATION_STYLE_ASSIGNMENT (( #5275 ) ) ;
#3924 = ORIENTED_EDGE ( 'NONE', *, *, #4214, .T. ) ;
#3925 = FACE_OUTER_BOUND ( 'NONE', #2296, .T. ) ;
#3926 = ORIENTED_EDGE ( 'NONE', *, *, #5052, .F. ) ;
#3927 = DIRECTION ( 'NONE',  ( 1.000000000000000000, 0.000000000000000000, 0.000000000000000000 ) ) ;
#3928 = CARTESIAN_POINT ( 'NONE',  ( -3.109042548464154621, -8.271822080921333864, 14.00000000000000000 ) ) ;
#3929 = CARTESIAN_POINT ( 'NONE',  ( -9.381622446298930385, -4.629808687489260777, 13.99999999999999645 ) ) ;
#3930 = AXIS2_PLACEMENT_3D ( 'NONE', #1303, #3061, #4803 ) ;
#3931 = ADVANCED_FACE ( 'NONE', ( #4261 ), #3401, .T. ) ;
#3932 = CARTESIAN_POINT ( 'NONE',  ( 0.000000000000000000, 0.000000000000000000, 5.000000000000000000 ) ) ;
#3933 = CARTESIAN_POINT ( 'NONE',  ( -5.081985621531964981, 6.397721742171718518, 14.00000000000000000 ) ) ;
#3934 = CIRCLE ( 'NONE', #1453, 0.2500000000000002220 ) ;
#3935 = EDGE_LOOP ( 'NONE', ( #5482, #3129, #485, #929 ) ) ;
#3936 = CARTESIAN_POINT ( 'NONE',  ( -0.7077576507783156501, 10.75210906117156995, 1.999999999999998224 ) ) ;
#3937 = CARTESIAN_POINT ( 'NONE',  ( -4.310533329765174670, 5.077046166955135220, 13.99999999999952927 ) ) ;
#3938 = CARTESIAN_POINT ( 'NONE',  ( 9.348788865897812883, 1.705571004836294646, 1.999999999999998224 ) ) ;
#3939 = EDGE_LOOP ( 'NONE', ( #4330, #1677, #2985, #3038 ) ) ;
#3940 = CARTESIAN_POINT ( 'NONE',  ( 7.025143070632193343, -0.1151745751371896220, 1.999999999999998224 ) ) ;
#3941 = CARTESIAN_POINT ( 'NONE',  ( 0.000000000000000000, 0.000000000000000000, -8.000000000000000000 ) ) ;
#3942 = CARTESIAN_POINT ( 'NONE',  ( -2.149999999999998579, 2.632990618166807756E-16, -3.106350832689629637 ) ) ;
#3943 = CARTESIAN_POINT ( 'NONE',  ( -5.183646570197097958, -3.010418922387011698, 1.999999999999998224 ) ) ;
#3944 = DIRECTION ( 'NONE',  ( 0.000000000000000000, 0.000000000000000000, 1.000000000000000000 ) ) ;
#3945 = ORIENTED_EDGE ( 'NONE', *, *, #2981, .T. ) ;
#3946 = CARTESIAN_POINT ( 'NONE',  ( 11.00000000000000355, -2.486888733138625796E-14, 7.999999999999996447 ) ) ;
#3947 = EDGE_CURVE ( 'NONE', #118, #4159, #1256, .T. ) ;
#3948 = CARTESIAN_POINT ( 'NONE',  ( -2.179108132477381332, -10.08557389312607278, 13.99999999999999645 ) ) ;
#3949 = CARTESIAN_POINT ( 'NONE',  ( 1.380000000000002336, 22.95856267278071172, 5.000000000000000888 ) ) ;
#3950 = ORIENTED_EDGE ( 'NONE', *, *, #1872, .T. ) ;
#3951 = DIRECTION ( 'NONE',  ( 1.000000000000000000, 0.000000000000000000, 0.000000000000000000 ) ) ;
#3952 = EDGE_LOOP ( 'NONE', ( #1700, #3632, #197, #3237 ) ) ;
#3953 = EDGE_LOOP ( 'NONE', ( #2284, #1392, #1290, #2323 ) ) ;
#3954 = CARTESIAN_POINT ( 'NONE',  ( 1.881113203117336319, 8.098457488330069509, 14.00000000000000000 ) ) ;
#3955 = CARTESIAN_POINT ( 'NONE',  ( -6.576488680450179203, -0.2289623203888876135, 1.999999999999998224 ) ) ;
#3956 = DIRECTION ( 'NONE',  ( 1.000000000000000000, 0.000000000000000000, 0.000000000000000000 ) ) ;
#3957 = CARTESIAN_POINT ( 'NONE',  ( 6.037635170864974477, 5.848285684831325604, 14.00000000000000000 ) ) ;
#3958 = ORIENTED_EDGE ( 'NONE', *, *, #224, .T. ) ;
#3959 = CARTESIAN_POINT ( 'NONE',  ( -9.381622446299669349, -4.629808687489259889, 1.999999999999998224 ) ) ;
#3960 = CARTESIAN_POINT ( 'NONE',  ( 10.20000000000000107, 0.000000000000000000, 1.610000000000000098 ) ) ;
#3961 = CARTESIAN_POINT ( 'NONE',  ( -0.5931392160223127874, -7.263020831007573896, 13.99999999999999645 ) ) ;
#3962 = APPLICATION_PROTOCOL_DEFINITION ( 'draft international standard', 'automotive_design', 1998, #3760 ) ;
#3963 = CARTESIAN_POINT ( 'NONE',  ( -1.515482495401827556, 9.129776367296644324, 1.999999999999998224 ) ) ;
#3964 = CARTESIAN_POINT ( 'NONE',  ( 1.015216742983932274, 7.730330528320553896, 1.999999999999998224 ) ) ;
#3965 = FACE_OUTER_BOUND ( 'NONE', #12, .T. ) ;
#3966 = EDGE_CURVE ( 'NONE', #2746, #4295, #2242, .T. ) ;
#3967 = DIRECTION ( 'NONE',  ( -0.000000000000000000, -0.4999999999999999445, -0.8660254037844387076 ) ) ;
#3968 = CARTESIAN_POINT ( 'NONE',  ( 5.460516619045266751, 3.400499599735594014, 1.999999999999998224 ) ) ;
#3969 = DIRECTION ( 'NONE',  ( -0.000000000000000000, -0.000000000000000000, -1.000000000000000000 ) ) ;
#3970 = EDGE_LOOP ( 'NONE', ( #4086, #4777, #2312 ) ) ;
#3971 = LINE ( 'NONE', #1388, #4201 ) ;
#3972 = CARTESIAN_POINT ( 'NONE',  ( 10.86297249782086105, 1.796588950249321304, 13.99999999999999645 ) ) ;
#3973 = EDGE_CURVE ( 'NONE', #4473, #4295, #2726, .T. ) ;
#3974 = SURFACE_STYLE_FILL_AREA ( #8 ) ;
#3975 = DIRECTION ( 'NONE',  ( 0.000000000000000000, 0.000000000000000000, -1.000000000000000000 ) ) ;
#3976 = ORIENTED_EDGE ( 'NONE', *, *, #3286, .T. ) ;
#3977 = ORIENTED_EDGE ( 'NONE', *, *, #93, .T. ) ;
#3978 = CARTESIAN_POINT ( 'NONE',  ( 5.612687125618119666, -6.603876269260188892, 14.00000000000000000 ) ) ;
#3979 = CARTESIAN_POINT ( 'NONE',  ( 5.103689747953258582, 6.014827819656408892, 1.999999999999998224 ) ) ;
#3980 = EDGE_CURVE ( 'NONE', #5536, #2168, #4651, .T. ) ;
#3981 = CARTESIAN_POINT ( 'NONE',  ( 2.400000000000000799, 0.000000000000000000, 0.000000000000000000 ) ) ;
#3982 = CARTESIAN_POINT ( 'NONE',  ( -1.001529162299639619, -8.740421795711004194, 14.00000000000000000 ) ) ;
#3983 = EDGE_CURVE ( 'NONE', #726, #247, #3075, .T. ) ;
#3984 = VERTEX_POINT ( 'NONE', #4889 ) ;
#3985 = CARTESIAN_POINT ( 'NONE',  ( 9.650319724628623419, 2.588775111615904567, 1.999999999999998224 ) ) ;
#3986=STYLED_ITEM('',(#5737),#4492);
#3987 = CARTESIAN_POINT ( 'NONE',  ( -4.892757975385434221, 9.527326283049751154, 1.999999999999998224 ) ) ;
#3988 = CARTESIAN_POINT ( 'NONE',  ( -6.576488680450180979, -0.2289623203888878078, 13.99999999999999645 ) ) ;
#3989 = TOROIDAL_SURFACE ( 'NONE', #2430, 2.199999999999999289, 0.2000000000000000111 ) ;
#3990 = CARTESIAN_POINT ( 'NONE',  ( 2.678407690932628871, -9.362678857629568085, 1.999999999999998224 ) ) ;
#3991 = CARTESIAN_POINT ( 'NONE',  ( 7.812003909081975728, 1.689803927524521354, 1.999999999999998224 ) ) ;
#3992 = DIRECTION ( 'NONE',  ( 0.06000000000000008105, 0.9981983770774224274, 0.000000000000000000 ) ) ;
#3993 = VECTOR ( 'NONE', #1355, 1000.000000000000000 ) ;
#3994 = CARTESIAN_POINT ( 'NONE',  ( 15.00000000000000000, 1.836970198721029589E-15, 12.00000000000000000 ) ) ;
#3995 =( LENGTH_UNIT ( ) NAMED_UNIT ( * ) SI_UNIT ( .MILLI., .METRE. ) );
#3996 = CARTESIAN_POINT ( 'NONE',  ( 8.774740126074938473, 5.663528079765400847, 1.999999999999998224 ) ) ;
#3997 = ADVANCED_FACE ( 'NONE', ( #28 ), #1813, .F. ) ;
#3998 = AXIS2_PLACEMENT_3D ( 'NONE', #317, #1993, #1070 ) ;
#3999 = DIRECTION ( 'NONE',  ( -0.000000000000000000, -0.000000000000000000, 1.000000000000000000 ) ) ;
#4000 = LINE ( 'NONE', #57, #2648 ) ;
#4001 = VERTEX_POINT ( 'NONE', #3598 ) ;
#4002 = PLANE ( 'NONE',  #2640 ) ;
#4003 = AXIS2_PLACEMENT_3D ( 'NONE', #1366, #1788, #3951 ) ;
#4004 = CARTESIAN_POINT ( 'NONE',  ( 3.605080641953931853, -9.570177220922108319, 13.99999999999999645 ) ) ;
#4005 = AXIS2_PLACEMENT_3D ( 'NONE', #4293, #1670, #2477 ) ;
#4006 = CARTESIAN_POINT ( 'NONE',  ( -1.380000000000000115, 22.95856267278071527, 1.371299631966804711 ) ) ;
#4007 = ORIENTED_EDGE ( 'NONE', *, *, #5268, .F. ) ;
#4008 = ORIENTED_EDGE ( 'NONE', *, *, #679, .T. ) ;
#4009 = CARTESIAN_POINT ( 'NONE',  ( -8.763921109941536614, 2.343993041296470903, 14.00000000000000000 ) ) ;
#4010 = CARTESIAN_POINT ( 'NONE',  ( -2.919577271296705412, -6.733962781534540198, 1.999999999999998224 ) ) ;
#4011 = EDGE_CURVE ( 'NONE', #2461, #586, #1441, .T. ) ;
#4012 = CIRCLE ( 'NONE', #5120, 2.000000000000000000 ) ;
#4013 = CARTESIAN_POINT ( 'NONE',  ( -6.281085993838467552, -4.827840781182768382, 1.999999999999998224 ) ) ;
#4014 = CARTESIAN_POINT ( 'NONE',  ( -3.109042548464154621, -8.271822080921333864, 14.00000000000000000 ) ) ;
#4015 = ORIENTED_EDGE ( 'NONE', *, *, #4934, .F. ) ;
#4016 = AXIS2_PLACEMENT_3D ( 'NONE', #2511, #3868, #380 ) ;
#4017 = CARTESIAN_POINT ( 'NONE',  ( -10.42442484909470046, -1.371544430045556373, 1.999999999999998224 ) ) ;
#4018 = CARTESIAN_POINT ( 'NONE',  ( 5.733165789232424814, 2.946509839760390381, 14.00000000000000000 ) ) ;
#4019 = CARTESIAN_POINT ( 'NONE',  ( -1.565980662507674648, 8.609317438862776228, 13.99999999999999645 ) ) ;
#4020 = CARTESIAN_POINT ( 'NONE',  ( -0.1359230501496729582, -8.279147739301068398, 13.99999999999999645 ) ) ;
#4021 = CIRCLE ( 'NONE', #1544, 22.50000000000000355 ) ;
#4022 = CONTEXT_DEPENDENT_SHAPE_REPRESENTATION ( #3871, #636 ) ;
#4023 = CARTESIAN_POINT ( 'NONE',  ( 5.059064342543293513, -7.053288479151686552, 1.999999999999998224 ) ) ;
#4024 = CARTESIAN_POINT ( 'NONE',  ( 4.793600759081159346, 4.956424179878264447, 1.999999999999998224 ) ) ;
#4025 = ADVANCED_FACE ( 'NONE', ( #5384 ), #434, .F. ) ;
#4026 = CIRCLE ( 'NONE', #1080, 5.000000000000000000 ) ;
#4027 = CARTESIAN_POINT ( 'NONE',  ( 11.00000000000000355, -2.486888733138625796E-14, 7.999999999999996447 ) ) ;
#4028 = FACE_OUTER_BOUND ( 'NONE', #2219, .T. ) ;
#4029 = CARTESIAN_POINT ( 'NONE',  ( 9.602236826901936695, 4.172718697305983326, 1.999999999999998224 ) ) ;
#4030 = CARTESIAN_POINT ( 'NONE',  ( -1.320393794063943416, 6.095439640211752774, 1.999999999999998224 ) ) ;
#4031 = DIRECTION ( 'NONE',  ( -0.000000000000000000, -0.000000000000000000, 1.000000000000000000 ) ) ;
#4032 = FACE_OUTER_BOUND ( 'NONE', #1124, .T. ) ;
#4033 = UNCERTAINTY_MEASURE_WITH_UNIT (LENGTH_MEASURE( 1.000000000000000082E-05 ), #314, 'distance_accuracy_value', 'NONE');
#4034 = EDGE_CURVE ( 'NONE', #3843, #2869, #2368, .T. ) ;
#4035 = CARTESIAN_POINT ( 'NONE',  ( -9.381622446298930385, -4.629808687489260777, 13.99999999999999645 ) ) ;
#4036 = DIRECTION ( 'NONE',  ( 1.000000000000000000, 0.000000000000000000, 0.000000000000000000 ) ) ;
#4037 = DIRECTION ( 'NONE',  ( -0.000000000000000000, -0.000000000000000000, -1.000000000000000000 ) ) ;
#4038 = ORIENTED_EDGE ( 'NONE', *, *, #105, .F. ) ;
#4039 = EDGE_LOOP ( 'NONE', ( #4942, #5464, #449, #4498 ) ) ;
#4040 = CARTESIAN_POINT ( 'NONE',  ( -8.332455577112462208, 5.761155596212925722, 14.00000000000000000 ) ) ;
#4041 = CARTESIAN_POINT ( 'NONE',  ( 7.132151089625187623, 3.519983721611797733, 1.999999999999998224 ) ) ;
#4042 = CARTESIAN_POINT ( 'NONE',  ( -3.987536574860945038, 7.161134007378406885, 1.999999999999998224 ) ) ;
#4043 = CARTESIAN_POINT ( 'NONE',  ( -8.547479018125100581, -2.754496926847988636, 14.00000000000000000 ) ) ;
#4044 = VERTEX_POINT ( 'NONE', #55 ) ;
#4045 = CARTESIAN_POINT ( 'NONE',  ( 7.233280636258586860, 6.778630567624379211, 1.999999999999998224 ) ) ;
#4046 = EDGE_CURVE ( 'NONE', #276, #5601, #1500, .T. ) ;
#4047 = DIRECTION ( 'NONE',  ( -0.000000000000000000, -1.000000000000000000, -0.000000000000000000 ) ) ;
#4048 = CARTESIAN_POINT ( 'NONE',  ( -8.486979168634645632, -0.6954046021538184963, 13.99999999999999645 ) ) ;
#4049 = CARTESIAN_POINT ( 'NONE',  ( 3.471913601335457233, 7.039518430846527508, 13.99999999999999645 ) ) ;
#4050 = CARTESIAN_POINT ( 'NONE',  ( 10.36702220812592223, 1.720931399333113676, 1.999999999999998224 ) ) ;
#4051 = CARTESIAN_POINT ( 'NONE',  ( -2.263950162103713915, 8.438937471999857109, 1.999999999999998224 ) ) ;
#4052 =( NAMED_UNIT ( * ) SI_UNIT ( $, .STERADIAN. ) SOLID_ANGLE_UNIT ( ) );
#4053 = ADVANCED_BREP_SHAPE_REPRESENTATION ( '', ( #4501, #1336 ), #3360 ) ;
#4054 = CARTESIAN_POINT ( 'NONE',  ( -1.500000000000000444, 24.95495942693556302, 1.371299631966804711 ) ) ;
#4055 = CARTESIAN_POINT ( 'NONE',  ( 6.496939485553420823, 0.4301729194711073623, 1.999999999999998224 ) ) ;
#4056 = ORIENTED_EDGE ( 'NONE', *, *, #1368, .T. ) ;
#4057 = DIRECTION ( 'NONE',  ( 0.000000000000000000, 0.000000000000000000, -1.000000000000000000 ) ) ;
#4058 = FACE_OUTER_BOUND ( 'NONE', #757, .T. ) ;
#4059 = EDGE_CURVE ( 'NONE', #5593, #928, #3620, .T. ) ;
#4060 = DIRECTION ( 'NONE',  ( 0.000000000000000000, 0.000000000000000000, 1.000000000000000000 ) ) ;
#4061 = ADVANCED_FACE ( 'NONE', ( #2675 ), #1408, .T. ) ;
#4062 = EDGE_CURVE ( 'NONE', #1449, #4872, #3480, .T. ) ;
#4063 = CARTESIAN_POINT ( 'NONE',  ( 5.099673838353210975, -8.834479793763010846, 13.99999999999999645 ) ) ;
#4064 =( LENGTH_UNIT ( ) NAMED_UNIT ( * ) SI_UNIT ( .MILLI., .METRE. ) );
#4065 = DIRECTION ( 'NONE',  ( -1.000000000000000000, 0.000000000000000000, 0.000000000000000000 ) ) ;
#4066 = EDGE_LOOP ( 'NONE', ( #1417, #3383, #3415, #865 ) ) ;
#4067 = EDGE_LOOP ( 'NONE', ( #618, #2383 ) ) ;
#4068 = CARTESIAN_POINT ( 'NONE',  ( -9.445900372710701376, 3.550092993115766760, 14.00000000000000000 ) ) ;
#4069 = CARTESIAN_POINT ( 'NONE',  ( -2.122668041763332347, 7.434468402752582250, 1.999999999999998224 ) ) ;
#4070 = CARTESIAN_POINT ( 'NONE',  ( -8.913799778910963312, 1.613954699392611047, 1.999999999999998224 ) ) ;
#4071 = CARTESIAN_POINT ( 'NONE',  ( -5.748891254250207083, -8.037420881458274380, 14.00000000000000000 ) ) ;
#4072 = EDGE_CURVE ( 'NONE', #1397, #5686, #861, .T. ) ;
#4073 = VERTEX_POINT ( 'NONE', #947 ) ;
#4074 = CARTESIAN_POINT ( 'NONE',  ( 0.1774200004017884857, 10.78715707688374614, 1.999999999999998224 ) ) ;
#4075 = LINE ( 'NONE', #1507, #4304 ) ;
#4076 = CARTESIAN_POINT ( 'NONE',  ( -6.681468852107525613, -5.130140014479350974, 13.99999999999999645 ) ) ;
#4077 = CARTESIAN_POINT ( 'NONE',  ( 2.389076732465380548, -5.237771676862081449, 14.00000000000000000 ) ) ;
#4078 = VECTOR ( 'NONE', #5297, 1000.000000000000000 ) ;
#4079 = ORIENTED_EDGE ( 'NONE', *, *, #4790, .F. ) ;
#4080 = CARTESIAN_POINT ( 'NONE',  ( 7.024953159363688471, -4.052930060063556716, 1.999999999999998224 ) ) ;
#4081 = AXIS2_PLACEMENT_3D ( 'NONE', #2744, #4434, #3630 ) ;
#4082 = PLANE ( 'NONE',  #5379 ) ;
#4083 =( NAMED_UNIT ( * ) SI_UNIT ( $, .STERADIAN. ) SOLID_ANGLE_UNIT ( ) );
#4084 = CARTESIAN_POINT ( 'NONE',  ( -5.416162817796314144, -4.301262981183148426, 1.999999999999998224 ) ) ;
#4085 = ADVANCED_FACE ( 'NONE', ( #457 ), #2216, .T. ) ;
#4086 = ORIENTED_EDGE ( 'NONE', *, *, #4657, .F. ) ;
#4087 = CARTESIAN_POINT ( 'NONE',  ( -4.184906021401388898, -5.457255036755482180, 1.999999999999998224 ) ) ;
#4088 = CIRCLE ( 'NONE', #5466, 27.00000000000000355 ) ;
#4089 = DIRECTION ( 'NONE',  ( -0.000000000000000000, -0.000000000000000000, 1.000000000000000000 ) ) ;
#4090 = EDGE_CURVE ( 'NONE', #3887, #2508, #2650, .T. ) ;
#4091 = SURFACE_SIDE_STYLE ('',( #1953 ) ) ;
#4092 = VECTOR ( 'NONE', #3836, 1000.000000000000000 ) ;
#4093 = CYLINDRICAL_SURFACE ( 'NONE', #2622, 3.799999999999999378 ) ;
#4094 = FILL_AREA_STYLE ('',( #4869 ) ) ;
#4095 = FACE_OUTER_BOUND ( 'NONE', #171, .T. ) ;
#4096 = VERTEX_POINT ( 'NONE', #516 ) ;
#4097 = AXIS2_PLACEMENT_3D ( 'NONE', #4615, #1569, #2889 ) ;
#4098 = DIRECTION ( 'NONE',  ( -0.000000000000000000, 1.000000000000000000, -0.000000000000000000 ) ) ;
#4099 = CARTESIAN_POINT ( 'NONE',  ( -5.748891254250207083, -8.037420881458274380, 14.00000000000000000 ) ) ;
#4100 = CARTESIAN_POINT ( 'NONE',  ( 5.862282306371745300, 6.688714470717011196, 1.999999999999998224 ) ) ;
#4101 = AXIS2_PLACEMENT_3D ( 'NONE', #1448, #2681, #5306 ) ;
#4102 = CARTESIAN_POINT ( 'NONE',  ( 1.853537052132013363, -8.546502713975391075, 1.999999999999998224 ) ) ;
#4103 = CARTESIAN_POINT ( 'NONE',  ( -8.290222237439158093, 3.747600907060152586, 14.00000000000000000 ) ) ;
#4104 = ORIENTED_EDGE ( 'NONE', *, *, #2473, .T. ) ;
#4105 = CARTESIAN_POINT ( 'NONE',  ( 7.456063200420987691, 7.959410280423138140, 1.999999999999998224 ) ) ;
#4106 = CARTESIAN_POINT ( 'NONE',  ( 1.730265954310492571, 6.073542049876724747, 14.00000000000000000 ) ) ;
#4107 = CARTESIAN_POINT ( 'NONE',  ( -5.921118896519415919, 6.318058289644736369, 13.99999999999999645 ) ) ;
#4108 = AXIS2_PLACEMENT_3D ( 'NONE', #2966, #725, #2129 ) ;
#4109 = EDGE_CURVE ( 'NONE', #1307, #2597, #543, .T. ) ;
#4110 = CARTESIAN_POINT ( 'NONE',  ( -3.139313036748680563, 9.741172307226465321, 1.999999999999998224 ) ) ;
#4111 = VECTOR ( 'NONE', #373, 1000.000000000000000 ) ;
#4112 = ORIENTED_EDGE ( 'NONE', *, *, #446, .F. ) ;
#4113 = CARTESIAN_POINT ( 'NONE',  ( 5.347643153870339283, -7.463670412152253242, 1.999999999999998224 ) ) ;
#4114 = VECTOR ( 'NONE', #2386, 1000.000000000000000 ) ;
#4115 = DIRECTION ( 'NONE',  ( -0.8571673007021134438, 1.049727191138619928E-16, 0.5150380749100523792 ) ) ;
#4116 = SHAPE_REPRESENTATION ( 'Spring Coil Unit', ( #1336 ), #2498 ) ;
#4117 = CARTESIAN_POINT ( 'NONE',  ( -2.744490807750914030, 5.556819979548925481, 1.999999999999998224 ) ) ;
#4118 = ORIENTED_EDGE ( 'NONE', *, *, #3405, .F. ) ;
#4119 = AXIS2_PLACEMENT_3D ( 'NONE', #662, #4089, #1985 ) ;
#4120 = CARTESIAN_POINT ( 'NONE',  ( 6.004028658818956643, -2.715480180205985583, 1.999999999999998224 ) ) ;
#4121 = DIRECTION ( 'NONE',  ( -1.000000000000000000, 0.000000000000000000, 0.000000000000000000 ) ) ;
#4122 = CARTESIAN_POINT ( 'NONE',  ( 22.99999999999999645, -8.485281374238580199, -8.000000000000000000 ) ) ;
#4123 = DIRECTION ( 'NONE',  ( -1.000000000000000000, -0.000000000000000000, -0.000000000000000000 ) ) ;
#4124 = CARTESIAN_POINT ( 'NONE',  ( 5.500000000000000000, 0.000000000000000000, 1.999999999999998224 ) ) ;
#4125 = ORIENTED_EDGE ( 'NONE', *, *, #1454, .T. ) ;
#4126 = CARTESIAN_POINT ( 'NONE',  ( 11.00000000000000355, -2.488243985854232676E-14, 13.99999999999999645 ) ) ;
#4127 = CARTESIAN_POINT ( 'NONE',  ( 2.678407690932720353, -9.362678857628843332, 14.00000000000000000 ) ) ;
#4128 = CARTESIAN_POINT ( 'NONE',  ( 4.683456943470878819, 7.530568860026273015, 1.999999999999998224 ) ) ;
#4129 = CARTESIAN_POINT ( 'NONE',  ( 8.477027301005913174, -1.108685663976167080, 1.999999999999998224 ) ) ;
#4130 = CARTESIAN_POINT ( 'NONE',  ( -3.672794075660814617, 8.451992513476522362, 14.00000000000000000 ) ) ;
#4131 = CARTESIAN_POINT ( 'NONE',  ( -25.00000000000000000, 0.000000000000000000, 0.000000000000000000 ) ) ;
#4132 = ORIENTED_EDGE ( 'NONE', *, *, #1094, .F. ) ;
#4133 = PLANE ( 'NONE',  #4847 ) ;
#4134 = CARTESIAN_POINT ( 'NONE',  ( 2.227988792049260702, 5.923272706910787555, 14.00000000000000000 ) ) ;
#4135 = CARTESIAN_POINT ( 'NONE',  ( -7.551678268146210016, 5.989845445213457964, 13.99999999999999645 ) ) ;
#4136 = CARTESIAN_POINT ( 'NONE',  ( 9.925004466820084303, 3.374327561486830884, 1.999999999999998224 ) ) ;
#4137 = VERTEX_POINT ( 'NONE', #4917 ) ;
#4138 = CARTESIAN_POINT ( 'NONE',  ( -0.3010823416051299772, -9.281161307073867661, 1.999999999999998224 ) ) ;
#4139 = CARTESIAN_POINT ( 'NONE',  ( -22.50000000000000355, 0.000000000000000000, 12.00000000000000000 ) ) ;
#4140 = SURFACE_SIDE_STYLE ('',( #630 ) ) ;
#4141 = CARTESIAN_POINT ( 'NONE',  ( 3.621982275015807051, -5.614208739972523787, 1.999999999999998224 ) ) ;
#4142 = EDGE_LOOP ( 'NONE', ( #1504, #4523, #3924, #4704 ) ) ;
#4143 = CARTESIAN_POINT ( 'NONE',  ( 7.526353627798827439, -0.2404185136226760222, 1.999999999999998224 ) ) ;
#4144 = LINE ( 'NONE', #1952, #3837 ) ;
#4145 = CARTESIAN_POINT ( 'NONE',  ( 0.000000000000000000, 0.000000000000000000, 12.00000000000000000 ) ) ;
#4146 = ADVANCED_FACE ( 'NONE', ( #3056 ), #978, .T. ) ;
#4147 = FACE_OUTER_BOUND ( 'NONE', #1570, .T. ) ;
#4148 = LINE ( 'NONE', #4579, #4994 ) ;
#4149 = DIRECTION ( 'NONE',  ( -1.000000000000000000, -0.000000000000000000, -0.000000000000000000 ) ) ;
#4150 = EDGE_LOOP ( 'NONE', ( #3834, #2013 ) ) ;
#4151 = DIRECTION ( 'NONE',  ( -0.000000000000000000, -0.000000000000000000, -1.000000000000000000 ) ) ;
#4152 = FACE_OUTER_BOUND ( 'NONE', #3019, .T. ) ;
#4153 = CARTESIAN_POINT ( 'NONE',  ( 5.933674912743041041, -6.989438080420770305, 1.999999999999998224 ) ) ;
#4154 = EDGE_CURVE ( 'NONE', #4844, #3499, #4632, .T. ) ;
#4155 = CARTESIAN_POINT ( 'NONE',  ( -2.122668041763332347, 7.434468402752584026, 13.99999999999999645 ) ) ;
#4156 = CARTESIAN_POINT ( 'NONE',  ( -5.391417556048331505, 8.653185861734561612, 1.999999999999998224 ) ) ;
#4157 = DIRECTION ( 'NONE',  ( 0.000000000000000000, 0.000000000000000000, 1.000000000000000000 ) ) ;
#4158 = DIRECTION ( 'NONE',  ( -4.364351673553916694E-15, 1.000000000000000000, 0.000000000000000000 ) ) ;
#4159 = VERTEX_POINT ( 'NONE', #3942 ) ;
#4160 = CARTESIAN_POINT ( 'NONE',  ( 5.400000000000002132, 26.45448922205832432, 12.00000000000000000 ) ) ;
#4161 = ADVANCED_FACE ( 'NONE', ( #3115 ), #3399, .F. ) ;
#4162 = CARTESIAN_POINT ( 'NONE',  ( 5.772253124442537242, -3.205917188173946997, 14.00000000000000000 ) ) ;
#4163 = CARTESIAN_POINT ( 'NONE',  ( -9.533152408061619454, 0.1566715252476607312, 13.99999999999999645 ) ) ;
#4164 = EDGE_CURVE ( 'NONE', #4608, #4001, #401, .T. ) ;
#4165 = CARTESIAN_POINT ( 'NONE',  ( 5.500000000000001776, 0.000000000000000000, 14.00000000000000000 ) ) ;
#4166 =( REPRESENTATION_RELATIONSHIP ('NONE','NONE', #4854, #953 ) REPRESENTATION_RELATIONSHIP_WITH_TRANSFORMATION ( #78 )SHAPE_REPRESENTATION_RELATIONSHIP( ) );
#4167 = ORIENTED_EDGE ( 'NONE', *, *, #1817, .T. ) ;
#4168 = CARTESIAN_POINT ( 'NONE',  ( -0.1462562576243746360, 8.775315755191545719, 1.999999999999998224 ) ) ;
#4169 = DIRECTION ( 'NONE',  ( -1.000000000000000000, -0.000000000000000000, -0.000000000000000000 ) ) ;
#4170 = EDGE_CURVE ( 'NONE', #3604, #1496, #5548, .T. ) ;
#4171 = CARTESIAN_POINT ( 'NONE',  ( -5.034899347481144538, -4.722558430572731503, 1.999999999999998224 ) ) ;
#4172 = ORIENTED_EDGE ( 'NONE', *, *, #4109, .T. ) ;
#4173 = CARTESIAN_POINT ( 'NONE',  ( 4.064490656457592443, -6.524520197619557926, 1.999999999999998224 ) ) ;
#4174 = FACE_OUTER_BOUND ( 'NONE', #4722, .T. ) ;
#4175 = DIRECTION ( 'NONE',  ( -0.000000000000000000, -0.000000000000000000, -1.000000000000000000 ) ) ;
#4176 = EDGE_CURVE ( 'NONE', #3586, #964, #3167, .T. ) ;
#4177 = B_SPLINE_SURFACE_WITH_KNOTS ( 'NONE', 1, 3, ( 
 ( #5437, #5062, #1492, #1471, #2824, #4576, #635, #2852, #1120, #200, #3627, #5386, #1444, #571, #2326, #2559, #3795, #773, #1582, #1612, #4207, #2994, #3370, #4288, #4319, #5552, #2526, #3341, #5125, #258, #4740, #2474, #2933, #3422, #1182, #343, #693, #5208, #4685, #4231, #4660, #368, #4710, #724, #1234, #4257, #2016, #5093, #806, #2961, #282, #745, #2497, #1266, #2097, #2126, #5607, #3880, #2039, #5635, #308, #2070, #3027, #3827, #5582, #1692, #5524, #1642, #3447, #2446, #3770, #3398, #1151, #3855, #2907, #5151, #1209, #5173, #1666, #4507, #102, #5342, #858, #2614, #4964, #3644, #4374, #1460, #1400, #3589, #4343, #394, #2155, #1887, #3161, #3911, #1727, #4908, #5427, #561, #5666, #1483, #4939, #1021, #2315, #537, #996, #4076, #76, #967, #504, #3216, #4048, #5240, #2725, #1917, #2342, #2261, #2779, #4107, #162, #3478, #1297, #4772, #4019, #1831, #129, #4477, #2287, #5401, #3053, #4797, #1858, #4534, #832, #3615, #5371, #1428, #3672, #3187, #2755, #590, #2584, #1547, #2894, #5542, #3302, #2841, #4594, #2491, #5022, #5051, #737, #1109, #1079, #2867, #4619, #678, #4647, #1598, #2432, #651, #2403, #4246, #4163, #1135, #5114, #217, #3329, #4135, #1972, #1048, #3358, #3726, #5485, #274, #4193, #714, #3240, #2055, #244, #2006, #1508, #2924, #1573, #3271, #3786, #3758, #4560, #1942, #1169, #5514, #5078, #2465, #4222, #3815, #2031, #4676, #297, #5570, #4988, #2810, #623, #2375, #189, #3696, #5453, #5255, #763, #359, #876, #3929, #5141, #4760, #2513, #3897, #5683, #3437, #2113, #416, #3041, #1287, #2574, #3870, #3413, #5165, #1741, #2174, #1226, #3496, #5622, #1682, #1200, #2949, #4702, #4360, #5194, #4277, #329, #1254, #2203, #4787 ),
 ( #1310, #4390, #2088, #2545, #3468, #3068, #4812, #2635, #3015, #445, #3847, #5598, #821, #3955, #1658, #846, #1630, #3389, #2979, #4728, #5654, #2602, #792, #4307, #4333, #382, #2143, #1713, #5229, #2281, #1419, #2334, #3180, #2717, #3608, #1764, #554, #5394, #4414, #3521, #5310, #3636, #1452, #2309, #14, #1371, #1015, #3153, #4930, #4874, #1794, #4527, #4010, #3583, #4469, #3210, #1825, #5336, #2773, #959, #3098, #931, #4500, #5281, #1338, #989, #581, #2749, #1394, #4846, #904, #4900, #4069, #528, #120, #2661, #1879, #468, #3550, #2226, #3979, #4958, #39, #4041, #96, #1851, #3126, #2685, #4440, #495, #2254, #67, #5363, #3233, #2801, #2023, #264, #4979, #5475, #5041, #236, #3348, #1476, #1909, #5445, #3666, #4213, #1159, #5420, #5013, #1994, #1127, #3777, #1589, #208, #5532, #1039, #4552, #1534, #5101, #613, #5506, #2914, #704, #4667, #729, #2421, #3749, #2365, #182, #4128, #4100, #3292, #153, #1499, #1934, #3689, #3262, #1961, #1071, #2833, #4584, #643, #2394, #2858, #4153, #3714, #1565, #4184, #1100, #4611, #3320, #670, #5068, #2883, #4638, #2454, #1620, #3803, #289, #2047, #1190, #2941, #5560, #4693, #3379, #5133, #2482, #4238, #5288, #4937, #2689, #3525, #4852, #4445, #2777, #3613, #3104, #4532, #2285, #2313, #5368, #3587, #4045, #1856, #3130, #502, #3985, #4505, #1398, #2667, #74, #4962, #5399, #45, #126, #1458, #3214, #1344, #908, #2207, #1800, #1375, #1426, #4879, #935, #3185, #4418, #472, #3557, #994, #3959, #2259, #5316, #4017, #1019, #1829, #5340, #3159, #4905, #965, #2753, #558, #2723, #4475, #535, #18, #100, #4074, #1885, #3642, #1770, #2231, #1505, #4105, #2891, #2373, #2839, #3327, #5020, #4191, #587 ) ),
 .UNSPECIFIED., .F., .F., .F.,
 ( 2, 2 ),
 ( 4, 2, 2, 2, 2, 2, 2, 2, 2, 2, 2, 2, 2, 2, 2, 2, 2, 2, 2, 2, 2, 2, 2, 2, 2, 2, 2, 2, 2, 2, 2, 2, 2, 2, 2, 2, 2, 2, 2, 2, 2, 2, 2, 2, 2, 2, 2, 2, 2, 2, 2, 2, 2, 2, 2, 2, 2, 2, 2, 2, 2, 2, 2, 2, 2, 2, 2, 2, 2, 2, 2, 2, 2, 2, 2, 2, 2, 2, 2, 2, 2, 2, 2, 2, 2, 2, 2, 2, 2, 2, 2, 2, 2, 2, 2, 2, 2, 2, 2, 2, 2, 2, 2, 2, 2, 2, 2, 2, 2, 2, 2, 2, 2, 2, 2, 2, 2, 2, 2, 2, 4 ),
 ( 0.000000000000000000, 0.4799999999999999822 ),
 ( 0.000000000000000000, 0.01562500000000000000, 0.03125000000000000000, 0.04687500000000000000, 0.06250000000000000000, 0.07812500000000000000, 0.09375000000000000000, 0.1093750000000000000, 0.1250000000000000000, 0.1328125000000000000, 0.1406250000000000000, 0.1484375000000000000, 0.1562500000000000000, 0.1640625000000000000, 0.1718750000000000000, 0.1796875000000000000, 0.1875000000000000000, 0.1953125000000000000, 0.2031250000000000000, 0.2109375000000000000, 0.2187500000000000000, 0.2265625000000000000, 0.2343750000000000000, 0.2421875000000000000, 0.2500000000000000000, 0.2578125000000000000, 0.2656250000000000000, 0.2734375000000000000, 0.2812500000000000000, 0.2890625000000000000, 0.2968750000000000000, 0.3046875000000000000, 0.3125000000000000000, 0.3203125000000000000, 0.3281250000000000000, 0.3359375000000000000, 0.3437500000000000000, 0.3515625000000000000, 0.3593750000000000000, 0.3671875000000000000, 0.3750000000000000000, 0.3828125000000000000, 0.3906250000000000000, 0.3984375000000000000, 0.4062500000000000000, 0.4140625000000000000, 0.4218750000000000000, 0.4296875000000000000, 0.4375000000000000000, 0.4453125000000000000, 0.4531250000000000000, 0.4609375000000000000, 0.4687500000000000000, 0.4765625000000000000, 0.4843750000000000000, 0.4921875000000000000, 0.5000000000000000000, 0.5078125000000000000, 0.5156250000000000000, 0.5234375000000000000, 0.5312500000000000000, 0.5390625000000000000, 0.5468750000000000000, 0.5546875000000000000, 0.5625000000000000000, 0.5703125000000000000, 0.5781250000000000000, 0.5859375000000000000, 0.5937500000000000000, 0.6015625000000000000, 0.6093750000000000000, 0.6171875000000000000, 0.6250000000000000000, 0.6328125000000000000, 0.6406250000000000000, 0.6484375000000000000, 0.6562500000000000000, 0.6640625000000000000, 0.6718750000000000000, 0.6796875000000000000, 0.6875000000000000000, 0.6953125000000000000, 0.7031250000000000000, 0.7109375000000000000, 0.7187500000000000000, 0.7265625000000000000, 0.7343750000000000000, 0.7421875000000000000, 0.7500000000000000000, 0.7578125000000000000, 0.7656250000000000000, 0.7734375000000000000, 0.7812500000000000000, 0.7890625000000000000, 0.7968750000000000000, 0.8046875000000000000, 0.8125000000000000000, 0.8203125000000000000, 0.8281250000000000000, 0.8359375000000000000, 0.8437500000000000000, 0.8515625000000000000, 0.8593750000000000000, 0.8671875000000000000, 0.8750000000000000000, 0.8828125000000000000, 0.8906250000000000000, 0.8984375000000000000, 0.9062500000000000000, 0.9140625000000000000, 0.9218750000000000000, 0.9296875000000000000, 0.9375000000000000000, 0.9453125000000000000, 0.9531250000000000000, 0.9609375000000000000, 0.9687500000000000000, 0.9765625000000000000, 0.9843750000000000000, 0.9921875000000000000, 1.000000000000000000 ),
 .UNSPECIFIED. ) ;
#4178 = DIRECTION ( 'NONE',  ( 0.000000000000000000, 0.000000000000000000, -1.000000000000000000 ) ) ;
#4179 = UNCERTAINTY_MEASURE_WITH_UNIT (LENGTH_MEASURE( 1.000000000000000082E-05 ), #310, 'distance_accuracy_value', 'NONE');
#4180 = DIRECTION ( 'NONE',  ( -1.000000000000000000, 0.000000000000000000, -0.000000000000000000 ) ) ;
#4181 = ORIENTED_EDGE ( 'NONE', *, *, #4072, .T. ) ;
#4182 = DIRECTION ( 'NONE',  ( -1.000000000000000000, -0.000000000000000000, -0.000000000000000000 ) ) ;
#4183 = DIRECTION ( 'NONE',  ( -1.000000000000000000, 0.000000000000000000, 0.000000000000000000 ) ) ;
#4184 = CARTESIAN_POINT ( 'NONE',  ( 3.388254439433305176, -8.575817650944026482, 1.999999999999998224 ) ) ;
#4185 = CARTESIAN_POINT ( 'NONE',  ( -3.441860715206332522, -7.602597312514155270, 13.99999999999999645 ) ) ;
#4186 = CARTESIAN_POINT ( 'NONE',  ( 8.269507991092027055, 6.356934974246627235, 14.00000000000000000 ) ) ;
#4188 = ORIENTED_EDGE ( 'NONE', *, *, #2557, .T. ) ;
#4187 = AXIS2_PLACEMENT_3D ( 'NONE', #2590, #1214, #4263 ) ;
#4189 = DIRECTION ( 'NONE',  ( 0.000000000000000000, 0.000000000000000000, -1.000000000000000000 ) ) ;
#4190 = EDGE_LOOP ( 'NONE', ( #627, #732, #3612, #4219 ) ) ;
#4191 = CARTESIAN_POINT ( 'NONE',  ( 10.98697916625148707, 0.8999353979983775176, 1.999999999999998224 ) ) ;
#4192 = CARTESIAN_POINT ( 'NONE',  ( -1.987635485262058577, 6.951293809708866789, 14.00000000000000000 ) ) ;
#4193 = CARTESIAN_POINT ( 'NONE',  ( -0.7976699882156008670, 9.736979168371714621, 13.99999999999999645 ) ) ;
#4194 = ADVANCED_FACE ( 'NONE', ( #5508 ), #2458, .F. ) ;
#4195 = AXIS2_PLACEMENT_3D ( 'NONE', #3409, #842, #5566 ) ;
#4196 = CARTESIAN_POINT ( 'NONE',  ( 4.062840028443491569, -5.287223670286397059, 14.00000000000000000 ) ) ;
#4197 = ORIENTED_EDGE ( 'NONE', *, *, #3321, .F. ) ;
#4198 = CIRCLE ( 'NONE', #2346, 23.00000000000000000 ) ;
#4199 = CARTESIAN_POINT ( 'NONE',  ( -10.53467355221071777, 0.3418899515810866485, 1.999999999999998224 ) ) ;
#4200 = FACE_OUTER_BOUND ( 'NONE', #271, .T. ) ;
#4201 = VECTOR ( 'NONE', #2193, 1000.000000000000000 ) ;
#4202 = CARTESIAN_POINT ( 'NONE',  ( 1.540339863274624577, 7.144097608501353669, 1.999999999999998224 ) ) ;
#4203 = ORIENTED_EDGE ( 'NONE', *, *, #5002, .F. ) ;
#4204 = CARTESIAN_POINT ( 'NONE',  ( -6.065725208710914806, -3.376743199310592747, 1.999999999999998224 ) ) ;
#4205 = CARTESIAN_POINT ( 'NONE',  ( 0.000000000000000000, 2.449293598294705428E-16, -1.999999999999999112 ) ) ;
#4206 = AXIS2_PLACEMENT_3D ( 'NONE', #4725, #4275, #2489 ) ;
#4207 = CARTESIAN_POINT ( 'NONE',  ( -2.466819000628047487, 6.242838961510106977, 13.99999999999999645 ) ) ;
#4208 = DIRECTION ( 'NONE',  ( -1.000000000000000000, -2.664535259100375697E-15, 0.000000000000000000 ) ) ;
#4209 = DIRECTION ( 'NONE',  ( 0.000000000000000000, 0.000000000000000000, 1.000000000000000000 ) ) ;
#4210 = ORIENTED_EDGE ( 'NONE', *, *, #4524, .T. ) ;
#4211 = CYLINDRICAL_SURFACE ( 'NONE', #4470, 2.000000000000000000 ) ;
#4212 = DIRECTION ( 'NONE',  ( -0.000000000000000000, -0.000000000000000000, 1.000000000000000000 ) ) ;
#4213 = CARTESIAN_POINT ( 'NONE',  ( -5.741039858921414663, -6.128965587877393872, 1.999999999999998224 ) ) ;
#4214 = EDGE_CURVE ( 'NONE', #5361, #1139, #3351, .T. ) ;
#4215 = CARTESIAN_POINT ( 'NONE',  ( 5.857810772706378621, -5.665644577056677456, 13.99999999999999645 ) ) ;
#4216 = CARTESIAN_POINT ( 'NONE',  ( 0.000000000000000000, 0.000000000000000000, 2.000000000000000000 ) ) ;
#4217 = ORIENTED_EDGE ( 'NONE', *, *, #2485, .F. ) ;
#4218 = LINE ( 'NONE', #2027, #4921 ) ;
#4219 = ORIENTED_EDGE ( 'NONE', *, *, #5677, .F. ) ;
#4220 = CARTESIAN_POINT ( 'NONE',  ( 1.300000000000000044, 0.7216878364870328300, 1.249999999999999778 ) ) ;
#4221 = CARTESIAN_POINT ( 'NONE',  ( -2.547213823411295319, 6.752160688201485961, 14.00000000000000000 ) ) ;
#4222 = CARTESIAN_POINT ( 'NONE',  ( 8.595497693524210447, -5.345940745659388149, 13.99999999999999645 ) ) ;
#4223 = CARTESIAN_POINT ( 'NONE',  ( 6.160418207306094018, 1.983851483784787373, 14.00000000000000000 ) ) ;
#4224 = EDGE_CURVE ( 'NONE', #5647, #4643, #2917, .T. ) ;
#4225 = ORIENTED_EDGE ( 'NONE', *, *, #1278, .F. ) ;
#4226 = CARTESIAN_POINT ( 'NONE',  ( 9.599547022228483328, -3.085197981542975310, 1.999999999999998224 ) ) ;
#4227 = PRODUCT ( 'outer cover 2', 'outer cover 2', '', ( #1833 ) ) ;
#4228 = DIRECTION ( 'NONE',  ( -0.000000000000000000, -0.000000000000000000, 1.000000000000000000 ) ) ;
#4229 = CARTESIAN_POINT ( 'NONE',  ( 5.053476174607396842, -5.757900651972986950, 1.999999999999998224 ) ) ;
#4230 = CARTESIAN_POINT ( 'NONE',  ( 22.50000000000000355, 2.755455298081545172E-15, 14.00000000000000000 ) ) ;
#4231 = CARTESIAN_POINT ( 'NONE',  ( 6.460119401626726265, -2.924461030940389783, 13.99999999999999645 ) ) ;
#4232 = EDGE_CURVE ( 'NONE', #1931, #11, #2514, .T. ) ;
#4233 = LINE ( 'NONE', #3858, #3824 ) ;
#4234 = DIRECTION ( 'NONE',  ( -0.5000000000000044409, 1.060575238724903587E-16, -0.8660254037844360431 ) ) ;
#4235 = VERTEX_POINT ( 'NONE', #3751 ) ;
#4236 = DIRECTION ( 'NONE',  ( 0.000000000000000000, 0.000000000000000000, -1.000000000000000000 ) ) ;
#4237 = CARTESIAN_POINT ( 'NONE',  ( 0.000000000000000000, 0.000000000000000000, 0.000000000000000000 ) ) ;
#4238 = CARTESIAN_POINT ( 'NONE',  ( -8.402144917908874078, 4.670158400850170644, 1.999999999999998224 ) ) ;
#4239 = CARTESIAN_POINT ( 'NONE',  ( 6.019515613300196577, 7.843576796802396167, 13.99999999999999645 ) ) ;
#4240 = CARTESIAN_POINT ( 'NONE',  ( -4.668631340267771712, 9.078485505802326827, 14.00000000000000000 ) ) ;
#4241 = VERTEX_POINT ( 'NONE', #1567 ) ;
#4242 = CARTESIAN_POINT ( 'NONE',  ( 23.00000000000000000, 2.816687638038912352E-15, 2.000000000000000000 ) ) ;
#4243 = ORIENTED_EDGE ( 'NONE', *, *, #2646, .F. ) ;
#4244 = DIRECTION ( 'NONE',  ( 0.000000000000000000, 0.000000000000000000, -1.000000000000000000 ) ) ;
#4245 = CARTESIAN_POINT ( 'NONE',  ( 1.540339863274486465, 7.144097608501355445, 14.00000000000000000 ) ) ;
#4246 = CARTESIAN_POINT ( 'NONE',  ( -9.500632974893353122, -0.6255030753161997525, 13.99999999999999645 ) ) ;
#4247 = EDGE_CURVE ( 'NONE', #4802, #1117, #859, .T. ) ;
#4248 = CARTESIAN_POINT ( 'NONE',  ( 7.320916985966520407, 1.587212364775818285, 14.00000000000000000 ) ) ;
#4249 = ORIENTED_EDGE ( 'NONE', *, *, #4629, .T. ) ;
#4250 = CARTESIAN_POINT ( 'NONE',  ( 2.810994617404584783, -9.846529629019117991, 1.999999999999998224 ) ) ;
#4251 = STYLED_ITEM ( 'NONE', ( #1518 ), #1651 ) ;
#4252 = DIRECTION ( 'NONE',  ( -0.000000000000000000, -0.000000000000000000, -1.000000000000000000 ) ) ;
#4253 = CARTESIAN_POINT ( 'NONE',  ( 0.000000000000000000, 0.000000000000000000, 0.000000000000000000 ) ) ;
#4254 = CARTESIAN_POINT ( 'NONE',  ( -5.081985621532272290, 6.397721742171409431, 1.999999999999998224 ) ) ;
#4255 = AXIS2_PLACEMENT_3D ( 'NONE', #3336, #279, #3366 ) ;
#4256 = CARTESIAN_POINT ( 'NONE',  ( -1.500000000000000888, 24.95495942693557012, 5.000000000000000888 ) ) ;
#4257 = CARTESIAN_POINT ( 'NONE',  ( 2.869471237997715640, -6.613103333303074649, 13.99999999999999645 ) ) ;
#4258 = PRODUCT_RELATED_PRODUCT_CATEGORY ( 'part', '', ( #4680 ) ) ;
#4259 = FILL_AREA_STYLE ('',( #4711 ) ) ;
#4260 = CARTESIAN_POINT ( 'NONE',  ( -10.03347820201762630, 0.3196629254998830660, 1.999999999999998224 ) ) ;
#4261 = FACE_OUTER_BOUND ( 'NONE', #3970, .T. ) ;
#4262 = VECTOR ( 'NONE', #3719, 1000.000000000000000 ) ;
#4263 = DIRECTION ( 'NONE',  ( 0.000000000000000000, 0.5000000000000002220, -0.8660254037844384856 ) ) ;
#4264 = ORIENTED_EDGE ( 'NONE', *, *, #2646, .T. ) ;
#4265 = DIRECTION ( 'NONE',  ( 0.000000000000000000, 0.000000000000000000, -1.000000000000000000 ) ) ;
#4266 = PLANE ( 'NONE',  #3998 ) ;
#4267 = VECTOR ( 'NONE', #2240, 1000.000000000000000 ) ;
#4268 = CARTESIAN_POINT ( 'NONE',  ( 4.683456943470878819, 7.530568860026274791, 13.99999999999999645 ) ) ;
#4269 = CARTESIAN_POINT ( 'NONE',  ( 1.300000000000000044, 0.000000000000000000, 0.000000000000000000 ) ) ;
#4270 = VERTEX_POINT ( 'NONE', #756 ) ;
#4271 = PRODUCT_DEFINITION_SHAPE ( 'NONE', 'NONE',  #5694 ) ;
#4272 = CARTESIAN_POINT ( 'NONE',  ( 17.99999999999999289, -15.01665741768121443, 8.000000000000000000 ) ) ;
#4273 = EDGE_CURVE ( 'NONE', #465, #5361, #489, .T. ) ;
#4274 = EDGE_LOOP ( 'NONE', ( #4581, #3819, #4596, #4818, #2798 ) ) ;
#4275 = DIRECTION ( 'NONE',  ( 0.000000000000000000, 0.000000000000000000, 1.000000000000000000 ) ) ;
#4276 = CARTESIAN_POINT ( 'NONE',  ( 2.161943361801395014, -6.363123982928430067, 14.00000000000000000 ) ) ;
#4277 = CARTESIAN_POINT ( 'NONE',  ( 10.06493078320225010, 4.366638945734137245, 13.99999999999999645 ) ) ;
#4278 =( GEOMETRIC_REPRESENTATION_CONTEXT ( 3 ) GLOBAL_UNCERTAINTY_ASSIGNED_CONTEXT ( ( #4033 ) ) GLOBAL_UNIT_ASSIGNED_CONTEXT ( ( #314, #5639, #2910 ) ) REPRESENTATION_CONTEXT ( 'NONE', 'WORKASPACE' ) );
#4279 =( GEOMETRIC_REPRESENTATION_CONTEXT ( 3 ) GLOBAL_UNCERTAINTY_ASSIGNED_CONTEXT ( ( #3771 ) ) GLOBAL_UNIT_ASSIGNED_CONTEXT ( ( #1268, #2934, #5095 ) ) REPRESENTATION_CONTEXT ( 'NONE', 'WORKASPACE' ) );
#4280 = CARTESIAN_POINT ( 'NONE',  ( 1.103627080440590547, -6.655442145117441477, 14.00000000000000000 ) ) ;
#4281 = ORIENTED_EDGE ( 'NONE', *, *, #2721, .F. ) ;
#4282 = CARTESIAN_POINT ( 'NONE',  ( -5.250997584835956467, 8.145342823910020513, 1.999999999999998224 ) ) ;
#4283 = EDGE_CURVE ( 'NONE', #465, #4301, #672, .T. ) ;
#4284 = DIRECTION ( 'NONE',  ( -0.000000000000000000, -0.000000000000000000, -1.000000000000000000 ) ) ;
#4285 = CARTESIAN_POINT ( 'NONE',  ( 5.528193227148988420, 6.314447692498917242, 1.999999999999998224 ) ) ;
#4286 = CIRCLE ( 'NONE', #515, 1.999999999999999556 ) ;
#4287 = DIRECTION ( 'NONE',  ( 0.000000000000000000, 0.000000000000000000, 1.000000000000000000 ) ) ;
#4288 = CARTESIAN_POINT ( 'NONE',  ( 0.2194671214740386012, 6.774136816532214667, 13.99999999999999645 ) ) ;
#4289 = AXIS2_PLACEMENT_3D ( 'NONE', #1907, #2856, #1992 ) ;
#4290 = PRESENTATION_STYLE_ASSIGNMENT (( #2072 ) ) ;
#4291 = CARTESIAN_POINT ( 'NONE',  ( -7.559400777704422758, -6.425066744314571920, 1.999999999999998224 ) ) ;
#4292 = AXIS2_PLACEMENT_3D ( 'NONE', #1525, #4604, #174 ) ;
#4293 = CARTESIAN_POINT ( 'NONE',  ( 0.000000000000000000, 0.000000000000000000, 4.000000000000003553 ) ) ;
#4294 = DIRECTION ( 'NONE',  ( -1.000000000000000000, 0.000000000000000000, 0.000000000000000000 ) ) ;
#4295 = VERTEX_POINT ( 'NONE', #4642 ) ;
#4296 = CARTESIAN_POINT ( 'NONE',  ( 1.820000000000000062, 0.000000000000000000, 0.000000000000000000 ) ) ;
#4297 = DIRECTION ( 'NONE',  ( 0.000000000000000000, 0.000000000000000000, 1.000000000000000000 ) ) ;
#4298 = VECTOR ( 'NONE', #5551, 1000.000000000000000 ) ;
#4299 = CARTESIAN_POINT ( 'NONE',  ( -4.679820741050984445, -8.111215689329295486, 13.99999999999999645 ) ) ;
#4300 = FACE_OUTER_BOUND ( 'NONE', #682, .T. ) ;
#4301 = VERTEX_POINT ( 'NONE', #731 ) ;
#4302 = LINE ( 'NONE', #3009, #3272 ) ;
#4303 = VERTEX_POINT ( 'NONE', #2025 ) ;
#4304 = VECTOR ( 'NONE', #161, 1000.000000000000000 ) ;
#4305 = DIRECTION ( 'NONE',  ( -0.000000000000000000, -0.000000000000000000, 1.000000000000000000 ) ) ;
#4306 = CARTESIAN_POINT ( 'NONE',  ( -4.895455514773497718, -6.178604150901620073, 14.00000000000000000 ) ) ;
#4307 = CARTESIAN_POINT ( 'NONE',  ( 0.2194671214740537279, 6.774136816532212890, 1.999999999999998224 ) ) ;
#4308 = PRODUCT_DEFINITION_CONTEXT ( 'detailed design', #894, 'design' ) ;
#4309 = CARTESIAN_POINT ( 'NONE',  ( 0.000000000000000000, 0.000000000000000000, -2.000000000000000000 ) ) ;
#4310 = CARTESIAN_POINT ( 'NONE',  ( -2.547213823411295319, 6.752160688201485961, 14.00000000000000000 ) ) ;
#4311 = ORIENTED_EDGE ( 'NONE', *, *, #1423, .F. ) ;
#4312 = EDGE_CURVE ( 'NONE', #4732, #586, #2884, .T. ) ;
#4313 = CARTESIAN_POINT ( 'NONE',  ( -9.406456921418630657, 1.708717176649225511, 1.999999999999998224 ) ) ;
#4314 = ADVANCED_FACE ( 'NONE', ( #2137 ), #1365, .T. ) ;
#4315 = CARTESIAN_POINT ( 'NONE',  ( 5.586635445632386343, -4.430858740432560339, 13.99999999999999645 ) ) ;
#4316 = DIRECTION ( 'NONE',  ( 1.000000000000000000, 0.000000000000000000, 0.000000000000000000 ) ) ;
#4317 = CARTESIAN_POINT ( 'NONE',  ( -2.020383375745208987, -7.552201994671270846, 1.999999999999998224 ) ) ;
#4318 = FACE_OUTER_BOUND ( 'NONE', #362, .T. ) ;
#4319 = CARTESIAN_POINT ( 'NONE',  ( 0.7762864403411009473, 6.746413643992396736, 13.99999999999999645 ) ) ;
#4320 = CARTESIAN_POINT ( 'NONE',  ( 4.264126983937991611, 9.433107915010285893, 1.999999999999998224 ) ) ;
#4321 = DIRECTION ( 'NONE',  ( -1.000000000000000000, 0.000000000000000000, 0.000000000000000000 ) ) ;
#4322 = FACE_OUTER_BOUND ( 'NONE', #700, .T. ) ;
#4323 = ORIENTED_EDGE ( 'NONE', *, *, #800, .T. ) ;
#4324 = CARTESIAN_POINT ( 'NONE',  ( -1.500000000000000444, 24.95495942693556302, 1.371299631966804711 ) ) ;
#4325 = CARTESIAN_POINT ( 'NONE',  ( 0.000000000000000000, 0.000000000000000000, 0.000000000000000000 ) ) ;
#4326 = CARTESIAN_POINT ( 'NONE',  ( -5.893815055328263774, 7.676334994785688259, 13.99999999999999645 ) ) ;
#4327 = CARTESIAN_POINT ( 'NONE',  ( 0.000000000000000000, 0.000000000000000000, -2.000000000000000000 ) ) ;
#4328 = ORIENTED_EDGE ( 'NONE', *, *, #1995, .T. ) ;
#4329 = DIRECTION ( 'NONE',  ( 0.000000000000000000, 0.000000000000000000, -1.000000000000000000 ) ) ;
#4330 = ORIENTED_EDGE ( 'NONE', *, *, #598, .F. ) ;
#4331 = CARTESIAN_POINT ( 'NONE',  ( 0.000000000000000000, 0.000000000000000000, 11.00000000000000000 ) ) ;
#4332 = CARTESIAN_POINT ( 'NONE',  ( 1.147089839255721166, -8.682979827542890661, 14.00000000000000000 ) ) ;
#4333 = CARTESIAN_POINT ( 'NONE',  ( 0.7762864403411611214, 6.746413643992394960, 1.999999999999998224 ) ) ;
#4334 = DIRECTION ( 'NONE',  ( 1.000000000000000000, 0.000000000000000000, 0.000000000000000000 ) ) ;
#4335 = CARTESIAN_POINT ( 'NONE',  ( 6.929006764466010715, 4.804313515625074693, 14.00000000000000000 ) ) ;
#4336 = VERTEX_POINT ( 'NONE', #3949 ) ;
#4337 = CARTESIAN_POINT ( 'NONE',  ( 9.199536834907135585, 5.930433524309127513, 1.999999999999998224 ) ) ;
#4338 = ADVANCED_FACE ( 'NONE', ( #2538 ), #5646, .T. ) ;
#4339 = CARTESIAN_POINT ( 'NONE',  ( 0.7762864403411009473, 6.746413643992396736, 13.99999999999999645 ) ) ;
#4340 = SHAPE_DEFINITION_REPRESENTATION ( #3306, #4854 ) ;
#4341 = CARTESIAN_POINT ( 'NONE',  ( -7.588772809867561087, -4.728083520432016407, 1.999999999999998224 ) ) ;
#4342 = CARTESIAN_POINT ( 'NONE',  ( -7.211577653563208123, 2.317451195016654530, 1.999999999999998224 ) ) ;
#4343 = CARTESIAN_POINT ( 'NONE',  ( 7.565999024956893138, -2.848076369834590338, 13.99999999999999645 ) ) ;
#4344 = EDGE_CURVE ( 'NONE', #1283, #5110, #3431, .T. ) ;
#4345 = DIRECTION ( 'NONE',  ( -1.000000000000000000, 0.000000000000000000, 0.000000000000000000 ) ) ;
#4346 = CARTESIAN_POINT ( 'NONE',  ( -6.398096652174580790, -7.548242073784104278, 1.999999999999998224 ) ) ;
#4347 = CARTESIAN_POINT ( 'NONE',  ( -2.199999999999999289, 2.694222958124176020E-16, -3.300000000000000266 ) ) ;
#4348 = DIRECTION ( 'NONE',  ( -0.000000000000000000, -0.000000000000000000, -1.000000000000000000 ) ) ;
#4349 = VERTEX_POINT ( 'NONE', #5187 ) ;
#4350 = CYLINDRICAL_SURFACE ( 'NONE', #520, 22.50000000000000355 ) ;
#4351 = ADVANCED_FACE ( 'NONE', ( #4300 ), #1246, .T. ) ;
#4352 = CARTESIAN_POINT ( 'NONE',  ( 4.043470907200354070, 7.877814422642792636, 13.99999999999999645 ) ) ;
#4353 = AXIS2_PLACEMENT_3D ( 'NONE', #1103, #4613, #815 ) ;
#4354 = PLANE ( 'NONE',  #769 ) ;
#4355 = ORIENTED_EDGE ( 'NONE', *, *, #916, .F. ) ;
#4356 = FACE_OUTER_BOUND ( 'NONE', #4039, .T. ) ;
#4357 = EDGE_LOOP ( 'NONE', ( #4782, #3865, #5509, #1258, #552 ) ) ;
#4358 = DIRECTION ( 'NONE',  ( 0.2000000000000000111, -0.9797958971132711969, -0.000000000000000000 ) ) ;
#4359 = CARTESIAN_POINT ( 'NONE',  ( 2.543939756934300966, 7.929199913827024382, 14.00000000000000000 ) ) ;
#4360 = CARTESIAN_POINT ( 'NONE',  ( 8.671201137382265500, 6.657490096169393468, 13.99999999999999645 ) ) ;
#4361 = VECTOR ( 'NONE', #3535, 1000.000000000000114 ) ;
#4362 = CARTESIAN_POINT ( 'NONE',  ( -1.500000000000000444, 24.95495942693556302, 11.00000000000000000 ) ) ;
#4363 = CARTESIAN_POINT ( 'NONE',  ( 8.370269057508139099, -1.803949267857856142, 14.00000000000000000 ) ) ;
#4364 = CIRCLE ( 'NONE', #2955, 12.50000000000000000 ) ;
#4365 = VECTOR ( 'NONE', #3552, 1000.000000000000000 ) ;
#4366 = EDGE_LOOP ( 'NONE', ( #5430, #4904, #4622, #4411, #4437, #3454, #5032, #99 ) ) ;
#4367 = DIRECTION ( 'NONE',  ( -4.364351673553916694E-15, 1.000000000000000000, 0.000000000000000000 ) ) ;
#4368 = VECTOR ( 'NONE', #5492, 1000.000000000000000 ) ;
#4369 = CARTESIAN_POINT ( 'NONE',  ( -7.375360291558942905, -1.341686286798741357, 13.99999999999999645 ) ) ;
#4370 = PRODUCT_CONTEXT ( 'NONE', #3760, 'mechanical' ) ;
#4371 = CARTESIAN_POINT ( 'NONE',  ( 9.522148329495122354, -0.6196525284525815636, 1.999999999999998224 ) ) ;
#4372 = VECTOR ( 'NONE', #915, 1000.000000000000000 ) ;
#4373 = CARTESIAN_POINT ( 'NONE',  ( -4.492165532403227246, -5.853844512260856447, 1.999999999999998224 ) ) ;
#4374 = CARTESIAN_POINT ( 'NONE',  ( 7.937472058415492526, 1.044590838406009858, 13.99999999999999645 ) ) ;
#4375 = DIRECTION ( 'NONE',  ( 0.000000000000000000, 0.000000000000000000, -1.000000000000000000 ) ) ;
#4376 = DIRECTION ( 'NONE',  ( 0.06000000000000008105, 0.9981983770774224274, 0.000000000000000000 ) ) ;
#4377 = CARTESIAN_POINT ( 'NONE',  ( -1.336592501075286599, -5.709464570123371274, 1.999999999999998224 ) ) ;
#4378 = CARTESIAN_POINT ( 'NONE',  ( -5.399999999999998579, 26.45448922205832787, 24.08672805191341482 ) ) ;
#4379 = ORIENTED_EDGE ( 'NONE', *, *, #6, .F. ) ;
#4380 = CIRCLE ( 'NONE', #330, 1.999999999999999556 ) ;
#4381 = CARTESIAN_POINT ( 'NONE',  ( 11.00000000000000355, -2.485533480423018915E-14, 1.999999999999998224 ) ) ;
#4382 = CARTESIAN_POINT ( 'NONE',  ( -0.7077576507784110182, 10.75210906117156995, 13.99999999999999645 ) ) ;
#4383 = VECTOR ( 'NONE', #60, 1000.000000000000000 ) ;
#4384 =( NAMED_UNIT ( * ) SI_UNIT ( $, .STERADIAN. ) SOLID_ANGLE_UNIT ( ) );
#4385 = ORIENTED_EDGE ( 'NONE', *, *, #585, .T. ) ;
#4386 = DIRECTION ( 'NONE',  ( 0.000000000000000000, 0.000000000000000000, 1.000000000000000000 ) ) ;
#4387 = ORIENTED_EDGE ( 'NONE', *, *, #4232, .T. ) ;
#4388 = ORIENTED_EDGE ( 'NONE', *, *, #5169, .T. ) ;
#4389 = CARTESIAN_POINT ( 'NONE',  ( -6.185289998984974780, -6.402116997106622520, 14.00000000000000000 ) ) ;
#4390 = CARTESIAN_POINT ( 'NONE',  ( 6.026041665150464688, -0.9817477132364114123, 1.999999999999998224 ) ) ;
#4391 = CARTESIAN_POINT ( 'NONE',  ( 0.000000000000000000, 0.000000000000000000, -8.000000000000000000 ) ) ;
#4392 = CARTESIAN_POINT ( 'NONE',  ( -7.945923533235638381, 1.308497053349305883, 14.00000000000000000 ) ) ;
#4393 = CIRCLE ( 'NONE', #5127, 23.00000000000000000 ) ;
#4394 = ORIENTED_EDGE ( 'NONE', *, *, #1405, .F. ) ;
#4395 = CARTESIAN_POINT ( 'NONE',  ( 10.06493078320224832, 4.366638945733749111, 1.999999999999998224 ) ) ;
#4396 = CARTESIAN_POINT ( 'NONE',  ( 3.909482108038855319, 5.648312977191786821, 13.99999999999999645 ) ) ;
#4397 = PRODUCT_CONTEXT ( 'NONE', #2768, 'mechanical' ) ;
#4398 = CARTESIAN_POINT ( 'NONE',  ( 9.123540010895986541, -2.926742269086382908, 1.999999999999998224 ) ) ;
#4399 = CARTESIAN_POINT ( 'NONE',  ( 5.194219494279652238, 4.554949839096303243, 1.999999999999998224 ) ) ;
#4400 = CARTESIAN_POINT ( 'NONE',  ( 0.000000000000000000, 0.000000000000000000, 14.00000000000000000 ) ) ;
#4401 = CARTESIAN_POINT ( 'NONE',  ( 1.300000000000000044, 0.7216878364870328300, 1.249999999999999778 ) ) ;
#4402 = CARTESIAN_POINT ( 'NONE',  ( 2.227988792049259814, 5.923272706911028251, 1.999999999999998224 ) ) ;
#4403 = LINE ( 'NONE', #435, #438 ) ;
#4404 = ORIENTED_EDGE ( 'NONE', *, *, #1716, .F. ) ;
#4405 = CARTESIAN_POINT ( 'NONE',  ( 5.500000000000000000, 0.000000000000000000, 1.999999999999998224 ) ) ;
#4406 = CARTESIAN_POINT ( 'NONE',  ( 0.000000000000000000, 0.000000000000000000, -5.000000000000000000 ) ) ;
#4407 = EDGE_CURVE ( 'NONE', #403, #4444, #3007, .T. ) ;
#4408 = DIRECTION ( 'NONE',  ( -1.000000000000000000, 0.000000000000000000, 0.000000000000000000 ) ) ;
#4409 = CARTESIAN_POINT ( 'NONE',  ( 0.000000000000000000, 0.000000000000000000, 0.000000000000000000 ) ) ;
#4410 = VERTEX_POINT ( 'NONE', #1758 ) ;
#4411 = ORIENTED_EDGE ( 'NONE', *, *, #2557, .F. ) ;
#4412 = CARTESIAN_POINT ( 'NONE',  ( 7.716263785693138644, -3.801003699433110228, 14.00000000000000000 ) ) ;
#4413 = EDGE_CURVE ( 'NONE', #5110, #1556, #2607, .T. ) ;
#4414 = CARTESIAN_POINT ( 'NONE',  ( 6.824478893064961582, -1.828844244265459329, 1.999999999999998224 ) ) ;
#4415 = CARTESIAN_POINT ( 'NONE',  ( 12.50000000000000000, 1.530808498934191521E-15, 2.000000000000000000 ) ) ;
#4416 = CARTESIAN_POINT ( 'NONE',  ( -0.1241967792452473573, -7.777596356722547455, 14.00000000000000000 ) ) ;
#4417 = ORIENTED_EDGE ( 'NONE', *, *, #5526, .T. ) ;
#4418 = CARTESIAN_POINT ( 'NONE',  ( -6.045729098460860484, -8.441868823237593134, 1.999999999999998224 ) ) ;
#4419 = FACE_OUTER_BOUND ( 'NONE', #2119, .T. ) ;
#4420 = EDGE_CURVE ( 'NONE', #5441, #1397, #5676, .T. ) ;
#4421 = CARTESIAN_POINT ( 'NONE',  ( 4.793600759081160234, 4.956424179878266223, 13.99999999999999645 ) ) ;
#4422 = ITEM_DEFINED_TRANSFORMATION ( 'NONE', 'NONE', #5447,  #1336 ) ;
#4423 = CARTESIAN_POINT ( 'NONE',  ( 4.853468040356245794, -8.397360160974407961, 1.999999999999998224 ) ) ;
#4424 = CARTESIAN_POINT ( 'NONE',  ( 6.997680802075242568, 0.4609939245310665235, 1.999999999999998224 ) ) ;
#4425 = PLANE ( 'NONE',  #1790 ) ;
#4426 = DIRECTION ( 'NONE',  ( -4.364351673553916694E-15, 1.000000000000000000, 0.000000000000000000 ) ) ;
#4427 = CARTESIAN_POINT ( 'NONE',  ( 3.896371052708264227, -4.167854722424304548, 1.999999999999998224 ) ) ;
#4428 = CARTESIAN_POINT ( 'NONE',  ( 6.315449825284093599, 1.474116854620456163, 1.999999999999998224 ) ) ;
#4429 = CARTESIAN_POINT ( 'NONE',  ( 1.300000000000000044, -0.7216878364870318308, -1.250000000000000000 ) ) ;
#4430 = ORIENTED_EDGE ( 'NONE', *, *, #3814, .T. ) ;
#4431 = EDGE_CURVE ( 'NONE', #1283, #1326, #5305, .T. ) ;
#4432 =( NAMED_UNIT ( * ) SI_UNIT ( $, .STERADIAN. ) SOLID_ANGLE_UNIT ( ) );
#4433 = CARTESIAN_POINT ( 'NONE',  ( 0.000000000000000000, 0.000000000000000000, 0.000000000000000000 ) ) ;
#4434 = DIRECTION ( 'NONE',  ( 0.000000000000000000, 0.000000000000000000, 1.000000000000000000 ) ) ;
#4435 = CARTESIAN_POINT ( 'NONE',  ( -1.379999999999999893, 22.95856267278071172, 15.94994774640597512 ) ) ;
#4436 =( GEOMETRIC_REPRESENTATION_CONTEXT ( 3 ) GLOBAL_UNCERTAINTY_ASSIGNED_CONTEXT ( ( #3042 ) ) GLOBAL_UNIT_ASSIGNED_CONTEXT ( ( #3419, #1663, #3877 ) ) REPRESENTATION_CONTEXT ( 'NONE', 'WORKASPACE' ) );
#4437 = ORIENTED_EDGE ( 'NONE', *, *, #3881, .F. ) ;
#4438 = ORIENTED_EDGE ( 'NONE', *, *, #4154, .T. ) ;
#4439 = CARTESIAN_POINT ( 'NONE',  ( 0.3244988297792451570, -9.772062696132405080, 14.00000000000000000 ) ) ;
#4440 = CARTESIAN_POINT ( 'NONE',  ( 7.992346231215205599, -0.9198489573344823533, 1.999999999999998224 ) ) ;
#4441 = CARTESIAN_POINT ( 'NONE',  ( -5.395431796987671724, -5.765308706272893602, 1.999999999999998224 ) ) ;
#4442 = ADVANCED_FACE ( 'NONE', ( #4752 ), #376, .T. ) ;
#4443 = CARTESIAN_POINT ( 'NONE',  ( -7.652305818843811558, 2.590529227167490234, 14.00000000000000000 ) ) ;
#4444 = VERTEX_POINT ( 'NONE', #1280 ) ;
#4445 = CARTESIAN_POINT ( 'NONE',  ( -3.127066335681005338, 9.214240776399423183, 1.999999999999998224 ) ) ;
#4446 = PRESENTATION_LAYER_ASSIGNMENT (  '', '', ( #5638 ) ) ;
#4447 = FACE_OUTER_BOUND ( 'NONE', #3698, .T. ) ;
#4448 = CARTESIAN_POINT ( 'NONE',  ( -5.210352092881700869, -6.569156856910654874, 13.99999999999999645 ) ) ;
#4449 = PRESENTATION_LAYER_ASSIGNMENT (  '', '', ( #3171 ) ) ;
#4450 = CARTESIAN_POINT ( 'NONE',  ( -8.763921109942213405, 2.343993041296470459, 1.999999999999998224 ) ) ;
#4451 = CARTESIAN_POINT ( 'NONE',  ( 3.471913601335177013, 7.039518430846525732, 1.999999999999998224 ) ) ;
#4452 = VECTOR ( 'NONE', #1928, 1000.000000000000000 ) ;
#4453 = CARTESIAN_POINT ( 'NONE',  ( 25.00000000000000000, -3.061616997868383043E-15, -8.000000000000000000 ) ) ;
#4454 =( NAMED_UNIT ( * ) PLANE_ANGLE_UNIT ( ) SI_UNIT ( $, .RADIAN. ) );
#4455 = CARTESIAN_POINT ( 'NONE',  ( 10.50003631213657762, 0.006025845833179020727, 1.999999999999998224 ) ) ;
#4456 = CIRCLE ( 'NONE', #4918, 1.249999999999999778 ) ;
#4457 = CARTESIAN_POINT ( 'NONE',  ( -3.987231204391976203, 4.693390172671164429, 1.999999999999412914 ) ) ;
#4458 = DIRECTION ( 'NONE',  ( 0.8571673007021134438, 0.000000000000000000, 0.5150380749100523792 ) ) ;
#4459 = ORIENTED_EDGE ( 'NONE', *, *, #4980, .T. ) ;
#4460 = CARTESIAN_POINT ( 'NONE',  ( 4.999999999999923617, 22.44994432064366308, 5.000000000000000000 ) ) ;
#4461 = AXIS2_PLACEMENT_3D ( 'NONE', #5018, #647, #1131 ) ;
#4462 = CARTESIAN_POINT ( 'NONE',  ( -6.726831604608805470, -7.927219868181097695, 13.99999999999999645 ) ) ;
#4463 = PRESENTATION_STYLE_ASSIGNMENT (( #549 ) ) ;
#4464 = CIRCLE ( 'NONE', #4101, 1.249999999999999778 ) ;
#4465 = FACE_OUTER_BOUND ( 'NONE', #3711, .T. ) ;
#4466 = ORIENTED_EDGE ( 'NONE', *, *, #5372, .F. ) ;
#4467 = VERTEX_POINT ( 'NONE', #3035 ) ;
#4468 = CARTESIAN_POINT ( 'NONE',  ( -9.692812185271368008, 2.758747493781260385, 14.00000000000000000 ) ) ;
#4469 = CARTESIAN_POINT ( 'NONE',  ( -4.492165532403227246, -5.853844512260856447, 1.999999999999998224 ) ) ;
#4470 = AXIS2_PLACEMENT_3D ( 'NONE', #262, #3775, #1474 ) ;
#4471 = CARTESIAN_POINT ( 'NONE',  ( -1.001529162299556797, -8.740421795711002417, 1.999999999999998224 ) ) ;
#4472 = CARTESIAN_POINT ( 'NONE',  ( -3.609299841826104416, -9.156952235374472338, 14.00000000000000000 ) ) ;
#4473 = VERTEX_POINT ( 'NONE', #4781 ) ;
#4474 = VECTOR ( 'NONE', #896, 1000.000000000000000 ) ;
#4475 = CARTESIAN_POINT ( 'NONE',  ( -4.892757975385434221, 9.527326283049751154, 1.999999999999998224 ) ) ;
#4476 = CARTESIAN_POINT ( 'NONE',  ( 5.526041665711820983, -0.8982374663919268087, 14.00000000000000000 ) ) ;
#4477 = CARTESIAN_POINT ( 'NONE',  ( 1.999247522871012483, 8.586038698135613600, 13.99999999999999645 ) ) ;
#4478 = CARTESIAN_POINT ( 'NONE',  ( 5.381714297850043849, -6.137309488907495947, 13.99999999999999645 ) ) ;
#4479 = AXIS2_PLACEMENT_3D ( 'NONE', #229, #5385, #173 ) ;
#4480 = EDGE_CURVE ( 'NONE', #3158, #964, #840, .T. ) ;
#4481 = CARTESIAN_POINT ( 'NONE',  ( -3.110890340275590304, -5.031137978950551037, 14.00000000000000000 ) ) ;
#4482 = MANIFOLD_SOLID_BREP ( 'Extrude-Thin2', #2546 ) ;
#4483 = CARTESIAN_POINT ( 'NONE',  ( 2.519353604429720228, -7.832629354751149187, 1.999999999999998224 ) ) ;
#4484 = ADVANCED_FACE ( 'NONE', ( #2276 ), #4354, .T. ) ;
#4485 = DIRECTION ( 'NONE',  ( -1.000000000000000000, 0.000000000000000000, 0.000000000000000000 ) ) ;
#4486 = CARTESIAN_POINT ( 'NONE',  ( 2.200000000000000622, 0.000000000000000000, 0.000000000000000000 ) ) ;
#4487 = CARTESIAN_POINT ( 'NONE',  ( 8.269507991092025279, 6.356934974247397285, 1.999999999999998224 ) ) ;
#4488 = VERTEX_POINT ( 'NONE', #5357 ) ;
#4489 = DIRECTION ( 'NONE',  ( 1.224646799147353207E-16, 1.000000000000000000, 0.000000000000000000 ) ) ;
#4490 = CARTESIAN_POINT ( 'NONE',  ( 0.000000000000000000, 0.000000000000000000, 8.000000000000000000 ) ) ;
#4491 = CARTESIAN_POINT ( 'NONE',  ( 0.000000000000000000, 0.000000000000000000, 8.000000000000000000 ) ) ;
#4492 = MANIFOLD_SOLID_BREP ( 'Extrude-Thin2', #1535 ) ;
#4493 = UNCERTAINTY_MEASURE_WITH_UNIT (LENGTH_MEASURE( 1.000000000000000082E-05 ), #5249, 'distance_accuracy_value', 'NONE');
#4494 = CARTESIAN_POINT ( 'NONE',  ( -1.342170334697156742, -10.21728332006373030, 13.99999999999999645 ) ) ;
#4495 = DIRECTION ( 'NONE',  ( 1.000000000000000000, 0.000000000000000000, -0.000000000000000000 ) ) ;
#4496 = DIRECTION ( 'NONE',  ( -1.156482317317871725E-16, -1.000000000000000000, 0.000000000000000000 ) ) ;
#4497 = ORIENTED_EDGE ( 'NONE', *, *, #4176, .T. ) ;
#4498 = ORIENTED_EDGE ( 'NONE', *, *, #1866, .T. ) ;
#4499 = CARTESIAN_POINT ( 'NONE',  ( -2.067895747887562141, -9.596367745172036834, 14.00000000000000000 ) ) ;
#4500 = CARTESIAN_POINT ( 'NONE',  ( -7.519441789400336695, 0.4931591957933217363, 1.999999999999998224 ) ) ;
#4501 = MANIFOLD_SOLID_BREP ( 'Cut-Extrude-Thin1', #5210 ) ;
#4502 = CARTESIAN_POINT ( 'NONE',  ( -8.757712506721389900, -2.046213373001789737, 1.999999999999998224 ) ) ;
#4503 = CARTESIAN_POINT ( 'NONE',  ( 3.433597602020987072, -9.098706718024024198, 14.00000000000000000 ) ) ;
#4504 = VERTEX_POINT ( 'NONE', #3602 ) ;
#4505 = CARTESIAN_POINT ( 'NONE',  ( 9.843274586260609027, 1.790275038161348364, 1.999999999999998224 ) ) ;
#4506 = DIRECTION ( 'NONE',  ( 0.000000000000000000, 0.000000000000000000, 1.000000000000000000 ) ) ;
#4507 = CARTESIAN_POINT ( 'NONE',  ( 4.585040342817689130, 6.402697129001494680, 13.99999999999999645 ) ) ;
#4508 = PRODUCT_RELATED_PRODUCT_CATEGORY ( 'part', '', ( #4589 ) ) ;
#4509 = ADVANCED_FACE ( 'NONE', ( #1874 ), #2248, .T. ) ;
#4510 = CARTESIAN_POINT ( 'NONE',  ( -6.708753103182418798, 7.642576097240645794, 1.999999999999998224 ) ) ;
#4511 = ORIENTED_EDGE ( 'NONE', *, *, #1888, .F. ) ;
#4512 = CARTESIAN_POINT ( 'NONE',  ( 8.164254108709977586, -4.026826083952141033, 1.999999999999998224 ) ) ;
#4513 = EDGE_CURVE ( 'NONE', #1194, #132, #1970, .T. ) ;
#4514 = LINE ( 'NONE', #1894, #691 ) ;
#4515 = CARTESIAN_POINT ( 'NONE',  ( -2.717942380035140104, -6.274577315194988181, 1.999999999999998224 ) ) ;
#4516 = VERTEX_POINT ( 'NONE', #176 ) ;
#4517 = CARTESIAN_POINT ( 'NONE',  ( -6.734745854535898246, 2.161492950161982396, 1.999999999999998224 ) ) ;
#4518 = CARTESIAN_POINT ( 'NONE',  ( -23.00000000000000000, 0.000000000000000000, 8.000000000000000000 ) ) ;
#4519 = FACE_BOUND ( 'NONE', #4067, .T. ) ;
#4520 =( NAMED_UNIT ( * ) PLANE_ANGLE_UNIT ( ) SI_UNIT ( $, .RADIAN. ) );
#4521 = CARTESIAN_POINT ( 'NONE',  ( 0.000000000000000000, 0.000000000000000000, -2.000000000000000000 ) ) ;
#4522 = DIRECTION ( 'NONE',  ( 1.000000000000000000, 0.000000000000000000, 0.000000000000000000 ) ) ;
#4523 = ORIENTED_EDGE ( 'NONE', *, *, #4273, .T. ) ;
#4524 = EDGE_CURVE ( 'NONE', #3046, #1815, #863, .T. ) ;
#4525 = LINE ( 'NONE', #702, #3006 ) ;
#4526 = CARTESIAN_POINT ( 'NONE',  ( 9.527640065891670673, 0.1642265212908743666, 14.00000000000000000 ) ) ;
#4527 = CARTESIAN_POINT ( 'NONE',  ( -2.352725117874390204, -6.938351456669183293, 1.999999999999998224 ) ) ;
#4528 = CARTESIAN_POINT ( 'NONE',  ( -7.963215149404742732, -4.094909132697305054, 1.999999999999998224 ) ) ;
#4529 = AXIS2_PLACEMENT_3D ( 'NONE', #5578, #2123, #4316 ) ;
#4530 = CARTESIAN_POINT ( 'NONE',  ( -10.03347820201837237, 0.3196629254998830660, 14.00000000000000000 ) ) ;
#4531 = ORIENTED_EDGE ( 'NONE', *, *, #800, .F. ) ;
#4532 = CARTESIAN_POINT ( 'NONE',  ( 1.598519525623709248, 9.677660462521251006, 1.999999999999998224 ) ) ;
#4533 = CARTESIAN_POINT ( 'NONE',  ( 4.513069810084764377, -3.445129632735343339, 14.00000000000000000 ) ) ;
#4534 = CARTESIAN_POINT ( 'NONE',  ( 7.344045208303976224, 5.086154276871550195, 13.99999999999999645 ) ) ;
#4535 = CARTESIAN_POINT ( 'NONE',  ( -8.929154442179981999, -4.413097966322209409, 1.999999999999998224 ) ) ;
#4536 = AXIS2_PLACEMENT_3D ( 'NONE', #1787, #34, #784 ) ;
#4537 = ORIENTED_EDGE ( 'NONE', *, *, #1524, .T. ) ;
#4538 = CARTESIAN_POINT ( 'NONE',  ( -8.440272934376206848, 1.393994921405934173, 1.999999999999998224 ) ) ;
#4539 = AXIS2_PLACEMENT_3D ( 'NONE', #2157, #3028, #3054 ) ;
#4540 = DIRECTION ( 'NONE',  ( -0.000000000000000000, -0.000000000000000000, 1.000000000000000000 ) ) ;
#4541 = CARTESIAN_POINT ( 'NONE',  ( -6.041022033915842471, 3.753782041846908779, 1.999999999999998224 ) ) ;
#4542 = ORIENTED_EDGE ( 'NONE', *, *, #2529, .T. ) ;
#4543 = CARTESIAN_POINT ( 'NONE',  ( 6.941605245898607279, 2.746080019686067519, 1.999999999999998224 ) ) ;
#4544 = VECTOR ( 'NONE', #3284, 1000.000000000000000 ) ;
#4545 = CARTESIAN_POINT ( 'NONE',  ( 1.820000000000000062, 0.000000000000000000, 0.000000000000000000 ) ) ;
#4546 = PRESENTATION_LAYER_ASSIGNMENT (  '', '', ( #5004 ) ) ;
#4547 = DIRECTION ( 'NONE',  ( -0.000000000000000000, -0.000000000000000000, 1.000000000000000000 ) ) ;
#4548 = ORIENTED_EDGE ( 'NONE', *, *, #5258, .T. ) ;
#4549 = CIRCLE ( 'NONE', #4003, 25.00000000000000000 ) ;
#4550 = CARTESIAN_POINT ( 'NONE',  ( 8.673617379884035472E-16, 0.000000000000000000, 0.000000000000000000 ) ) ;
#4551 = CARTESIAN_POINT ( 'NONE',  ( -7.966005157978615969, 4.422220743486623640, 14.00000000000000000 ) ) ;
#4552 = CARTESIAN_POINT ( 'NONE',  ( -7.245889760505162869, 4.668767092638087313, 1.999999999999998224 ) ) ;
#4553 = VECTOR ( 'NONE', #3425, 1000.000000000000000 ) ;
#4554 = CARTESIAN_POINT ( 'NONE',  ( -5.081985621532272290, 6.397721742171409431, 1.999999999999998224 ) ) ;
#4555 = CARTESIAN_POINT ( 'NONE',  ( -8.929154442179243034, -4.413097966322579779, 14.00000000000000000 ) ) ;
#4556 = CARTESIAN_POINT ( 'NONE',  ( -5.000000000000076383, 22.44994432064363110, 8.000000000000000000 ) ) ;
#4557 = ORIENTED_EDGE ( 'NONE', *, *, #23, .F. ) ;
#4558 = FACE_OUTER_BOUND ( 'NONE', #3213, .T. ) ;
#4559 = CARTESIAN_POINT ( 'NONE',  ( -3.110890340275590304, -5.031137978950551037, 14.00000000000000000 ) ) ;
#4560 = CARTESIAN_POINT ( 'NONE',  ( 9.843274586260610803, 1.790275038161259991, 13.99999999999999645 ) ) ;
#4561 = AXIS2_PLACEMENT_3D ( 'NONE', #5301, #87, #31 ) ;
#4562 = CARTESIAN_POINT ( 'NONE',  ( -3.609299841826103972, -9.156952235374472338, 1.999999999999998224 ) ) ;
#4563 = AXIS2_PLACEMENT_3D ( 'NONE', #2053, #4244, #1656 ) ;
#4564 = ORIENTED_EDGE ( 'NONE', *, *, #4344, .F. ) ;
#4565 = EDGE_CURVE ( 'NONE', #1556, #5110, #2610, .T. ) ;
#4566 = CARTESIAN_POINT ( 'NONE',  ( -1.565980662507674426, 8.609317438863394401, 1.999999999999998224 ) ) ;
#4567 = AXIS2_PLACEMENT_3D ( 'NONE', #804, #3397, #2125 ) ;
#4568 = DIRECTION ( 'NONE',  ( -3.540989467475305966E-16, -1.000000000000000000, 0.000000000000000000 ) ) ;
#4569 =( NAMED_UNIT ( * ) PLANE_ANGLE_UNIT ( ) SI_UNIT ( $, .RADIAN. ) );
#4570 = CARTESIAN_POINT ( 'NONE',  ( 4.443413384189978110, 4.597174039215664365, 1.999999999999998224 ) ) ;
#4571 = ORIENTED_EDGE ( 'NONE', *, *, #1423, .T. ) ;
#4572 = CIRCLE ( 'NONE', #1363, 2.199999999999999289 ) ;
#4573 = CARTESIAN_POINT ( 'NONE',  ( -1.987635485262058133, 6.951293809708865012, 1.999999999999998224 ) ) ;
#4574 = CARTESIAN_POINT ( 'NONE',  ( 1.300000000000000044, 1.443375672974065216, 7.017607234860990640E-28 ) ) ;
#4575 = EDGE_CURVE ( 'NONE', #1283, #4764, #127, .T. ) ;
#4576 = CARTESIAN_POINT ( 'NONE',  ( 2.597146444261842824, -5.700021143261160717, 13.99999999999999645 ) ) ;
#4577 = DIRECTION ( 'NONE',  ( 0.000000000000000000, 0.000000000000000000, -1.000000000000000000 ) ) ;
#4578 = EDGE_CURVE ( 'NONE', #3011, #30, #3901, .T. ) ;
#4579 = CARTESIAN_POINT ( 'NONE',  ( 22.99999999999999645, -8.485281374238580199, 8.000000000000000000 ) ) ;
#4580 = CARTESIAN_POINT ( 'NONE',  ( 25.00000000000000000, 3.061616997868383043E-15, 8.000000000000000000 ) ) ;
#4581 = ORIENTED_EDGE ( 'NONE', *, *, #2197, .T. ) ;
#4582 = CARTESIAN_POINT ( 'NONE',  ( 4.336808689942017736E-16, 0.000000000000000000, 0.000000000000000000 ) ) ;
#4583 = CARTESIAN_POINT ( 'NONE',  ( 17.74999999999999289, -15.01665741768121443, -8.000000000000000000 ) ) ;
#4584 = CARTESIAN_POINT ( 'NONE',  ( 8.454926800554316557, -3.338224220245900042, 1.999999999999998224 ) ) ;
#4585 = EDGE_CURVE ( 'NONE', #4844, #2131, #576, .T. ) ;
#4586 = CARTESIAN_POINT ( 'NONE',  ( -8.126042061586270293, 2.755650963504471473, 13.99999999999999645 ) ) ;
#4587 = CARTESIAN_POINT ( 'NONE',  ( 8.618507686538960044, 3.909830026711944573, 1.999999999999998224 ) ) ;
#4588 = CARTESIAN_POINT ( 'NONE',  ( -5.592500163774714039, 7.275211197852027745, 14.00000000000000000 ) ) ;
#4589 = PRODUCT ( 'Lock Button', 'Lock Button', '', ( #855 ) ) ;
#4590 = CARTESIAN_POINT ( 'NONE',  ( -25.00000000000000000, 0.000000000000000000, 0.000000000000000000 ) ) ;
#4591 = EDGE_LOOP ( 'NONE', ( #2653, #3 ) ) ;
#4592 = DIRECTION ( 'NONE',  ( 1.000000000000000000, 0.000000000000000000, -0.000000000000000000 ) ) ;
#4593 = CARTESIAN_POINT ( 'NONE',  ( 6.445330636073146380, -1.168293168414177741, 14.00000000000000000 ) ) ;
#4594 = CARTESIAN_POINT ( 'NONE',  ( 3.388254439433305176, -8.575817650944683734, 13.99999999999999645 ) ) ;
#4595 = CARTESIAN_POINT ( 'NONE',  ( -5.391417556048331505, 8.653185861734561612, 1.999999999999998224 ) ) ;
#4596 = ORIENTED_EDGE ( 'NONE', *, *, #149, .T. ) ;
#4597 = CARTESIAN_POINT ( 'NONE',  ( 2.701324588234195190, 8.405562337868014211, 1.999999999999998224 ) ) ;
#4598 = EDGE_CURVE ( 'NONE', #1755, #3693, #40, .T. ) ;
#4599 = PLANE ( 'NONE',  #4726 ) ;
#4600 = CARTESIAN_POINT ( 'NONE',  ( 1.103627080440590102, -6.655442145117440589, 1.999999999999998224 ) ) ;
#4601 = ORIENTED_EDGE ( 'NONE', *, *, #3071, .T. ) ;
#4602 = CARTESIAN_POINT ( 'NONE',  ( 6.340368144647110071, -1.697206311170896598, 1.999999999999998224 ) ) ;
#4603 = CARTESIAN_POINT ( 'NONE',  ( 1.300000000000000044, -0.7216878364870318308, 1.249999999999999778 ) ) ;
#4604 = DIRECTION ( 'NONE',  ( -0.000000000000000000, -0.000000000000000000, 1.000000000000000000 ) ) ;
#4605 = DIRECTION ( 'NONE',  ( 0.000000000000000000, 0.000000000000000000, 1.000000000000000000 ) ) ;
#4606 = EDGE_CURVE ( 'NONE', #5617, #5155, #4148, .T. ) ;
#4607 = DIRECTION ( 'NONE',  ( -1.000000000000000000, 0.000000000000000000, 0.000000000000000000 ) ) ;
#4608 = VERTEX_POINT ( 'NONE', #202 ) ;
#4609 = DIRECTION ( 'NONE',  ( -1.000000000000000000, 0.000000000000000000, -0.000000000000000000 ) ) ;
#4610 = CARTESIAN_POINT ( 'NONE',  ( 7.108868828250529681, 7.597268273415099138, 14.00000000000000000 ) ) ;
#4611 = CARTESIAN_POINT ( 'NONE',  ( 1.208067634251008604, -9.180948453718620783, 1.999999999999998224 ) ) ;
#4612 = CARTESIAN_POINT ( 'NONE',  ( -7.245889760505164645, 4.668767092638694827, 13.99999999999999645 ) ) ;
#4613 = DIRECTION ( 'NONE',  ( 0.000000000000000000, 0.000000000000000000, 1.000000000000000000 ) ) ;
#4614 = ORIENTED_EDGE ( 'NONE', *, *, #3638, .T. ) ;
#4615 = CARTESIAN_POINT ( 'NONE',  ( 0.000000000000000000, 0.000000000000000000, 2.000000000000000000 ) ) ;
#4616 = ORIENTED_EDGE ( 'NONE', *, *, #3745, .F. ) ;
#4617 = LINE ( 'NONE', #676, #5577 ) ;
#4618 = CARTESIAN_POINT ( 'NONE',  ( 5.499810765991187012, -5.314180015047230476, 14.00000000000000000 ) ) ;
#4619 = CARTESIAN_POINT ( 'NONE',  ( -5.337360893036674270, -7.710592058383929803, 13.99999999999999645 ) ) ;
#4620 = ADVANCED_FACE ( 'NONE', ( #2827 ), #1956, .T. ) ;
#4621 = CARTESIAN_POINT ( 'NONE',  ( 6.496939485553422600, 0.4301729194711386151, 14.00000000000000000 ) ) ;
#4622 = ORIENTED_EDGE ( 'NONE', *, *, #2567, .T. ) ;
#4623 = CARTESIAN_POINT ( 'NONE',  ( -3.798941939731882655, -9.621416145858376012, 1.999999999999998224 ) ) ;
#4624 = DIRECTION ( 'NONE',  ( -1.000000000000000000, 0.000000000000000000, 0.000000000000000000 ) ) ;
#4625 = SURFACE_SIDE_STYLE ('',( #2470 ) ) ;
#4626 = CARTESIAN_POINT ( 'NONE',  ( 2.672042568001582019, -6.151894458593051063, 1.999999999999998224 ) ) ;
#4627 = VERTEX_POINT ( 'NONE', #5284 ) ;
#4628 = CARTESIAN_POINT ( 'NONE',  ( -5.370374743918785221, 4.702532619530842339, 1.999999999999998224 ) ) ;
#4629 = EDGE_CURVE ( 'NONE', #276, #2517, #1340, .T. ) ;
#4630 = DIRECTION ( 'NONE',  ( 1.000000000000000000, 0.000000000000000000, 0.000000000000000000 ) ) ;
#4631 = CYLINDRICAL_SURFACE ( 'NONE', #1536, 13.00000000000000178 ) ;
#4632 = CIRCLE ( 'NONE', #4714, 25.00000000000000000 ) ;
#4633 = AXIS2_PLACEMENT_3D ( 'NONE', #4309, #418, #447 ) ;
#4634 = DIRECTION ( 'NONE',  ( -1.000000000000000000, -0.000000000000000000, -0.000000000000000000 ) ) ;
#4635 = ORIENTED_EDGE ( 'NONE', *, *, #328, .F. ) ;
#4636 = CARTESIAN_POINT ( 'NONE',  ( 0.000000000000000000, 0.000000000000000000, 8.000000000000000000 ) ) ;
#4637 = CARTESIAN_POINT ( 'NONE',  ( 0.000000000000000000, 0.000000000000000000, 11.00000000000000000 ) ) ;
#4638 = CARTESIAN_POINT ( 'NONE',  ( -4.679820741051314847, -8.111215689328634681, 1.999999999999998224 ) ) ;
#4639 = VECTOR ( 'NONE', #1093, 1000.000000000000114 ) ;
#4640 = ADVANCED_FACE ( 'NONE', ( #2116 ), #3899, .T. ) ;
#4641 = CARTESIAN_POINT ( 'NONE',  ( -3.845892476879857469, 6.661954734853424043, 13.99999999999999645 ) ) ;
#4642 = CARTESIAN_POINT ( 'NONE',  ( 2.149999999999998579, 0.000000000000000000, -3.106350832689629637 ) ) ;
#4643 = VERTEX_POINT ( 'NONE', #823 ) ;
#4644 = CARTESIAN_POINT ( 'NONE',  ( 0.000000000000000000, 0.000000000000000000, 12.00000000000000000 ) ) ;
#4645 = EDGE_LOOP ( 'NONE', ( #1736, #4172, #5259, #3274, #4671 ) ) ;
#4646 = CARTESIAN_POINT ( 'NONE',  ( -4.089163901200158158, 5.898691170884823975, 14.00000000000000000 ) ) ;
#4647 = CARTESIAN_POINT ( 'NONE',  ( -7.080399483669658878, -6.208478756603783566, 13.99999999999999645 ) ) ;
#4648 = CIRCLE ( 'NONE', #1247, 22.50000000000000355 ) ;
#4649 = CARTESIAN_POINT ( 'NONE',  ( -0.2403693791185868289, 7.265099133626555350, 14.00000000000000000 ) ) ;
#4650 = ORIENTED_EDGE ( 'NONE', *, *, #3227, .T. ) ;
#4651 = CIRCLE ( 'NONE', #2175, 25.00000000000000000 ) ;
#4652 = CARTESIAN_POINT ( 'NONE',  ( -9.247243397276459831, 2.478494142799053446, 1.999999999999998224 ) ) ;
#4653 = EDGE_CURVE ( 'NONE', #5601, #4073, #3470, .T. ) ;
#4654 = PLANE ( 'NONE',  #499 ) ;
#4655 = AXIS2_PLACEMENT_3D ( 'NONE', #5099, #1157, #4236 ) ;
#4656 = CARTESIAN_POINT ( 'NONE',  ( -1.390902631672706002, -7.679604985168658970, 1.999999999999998224 ) ) ;
#4657 = EDGE_CURVE ( 'NONE', #1449, #1931, #385, .T. ) ;
#4658 = CARTESIAN_POINT ( 'NONE',  ( -0.1241967792452471353, -7.777596356722545679, 1.999999999999998224 ) ) ;
#4659 = CARTESIAN_POINT ( 'NONE',  ( 4.999999999999914735, 24.49489742783179835, 5.000000000000000000 ) ) ;
#4660 = CARTESIAN_POINT ( 'NONE',  ( 6.209839678909983895, -3.451293940533043614, 13.99999999999999645 ) ) ;
#4661 = CARTESIAN_POINT ( 'NONE',  ( 0.000000000000000000, 0.000000000000000000, 0.000000000000000000 ) ) ;
#4662 = AXIS2_PLACEMENT_3D ( 'NONE', #4890, #3059, #864 ) ;
#4663 = DIRECTION ( 'NONE',  ( -0.000000000000000000, -0.000000000000000000, 1.000000000000000000 ) ) ;
#4664 = EDGE_LOOP ( 'NONE', ( #1489, #1367, #1625, #4281 ) ) ;
#4665 = CARTESIAN_POINT ( 'NONE',  ( -5.000000000000076383, 22.44994432064363110, -5.000000000000000000 ) ) ;
#4666 = CARTESIAN_POINT ( 'NONE',  ( 2.400000000000000799, 0.000000000000000000, 0.000000000000000000 ) ) ;
#4667 = CARTESIAN_POINT ( 'NONE',  ( -1.565980662507674426, 8.609317438863394401, 1.999999999999998224 ) ) ;
#4668 = EDGE_CURVE ( 'NONE', #3088, #4697, #2227, .T. ) ;
#4669 = CARTESIAN_POINT ( 'NONE',  ( 8.164254108709979363, -4.026826083952141921, 13.99999999999999645 ) ) ;
#4670 = CARTESIAN_POINT ( 'NONE',  ( 0.000000000000000000, 0.000000000000000000, 4.000000000000000000 ) ) ;
#4671 = ORIENTED_EDGE ( 'NONE', *, *, #5090, .F. ) ;
#4672 = CARTESIAN_POINT ( 'NONE',  ( 10.50003631213657407, 0.006025845833178966951, 1.999999999999998668 ) ) ;
#4673 = EDGE_LOOP ( 'NONE', ( #1485, #3976, #5611, #4614 ) ) ;
#4674 = CARTESIAN_POINT ( 'NONE',  ( 4.500000000000000888, 0.000000000000000000, 0.000000000000000000 ) ) ;
#4675 = CARTESIAN_POINT ( 'NONE',  ( 4.064490656458173312, -6.524520197619847472, 14.00000000000000000 ) ) ;
#4676 = CARTESIAN_POINT ( 'NONE',  ( 5.800093669798302543, -8.375184749302979625, 13.99999999999999645 ) ) ;
#4677 = CARTESIAN_POINT ( 'NONE',  ( 6.941605245898609056, 2.746080019685927187, 14.00000000000000000 ) ) ;
#4678 = ORIENTED_EDGE ( 'NONE', *, *, #2950, .F. ) ;
#4679 = CARTESIAN_POINT ( 'NONE',  ( 9.843274586260609027, 1.790275038161348364, 1.999999999999998224 ) ) ;
#4680 = PRODUCT ( 'TAS-001', 'TAS-001', '', ( #1348 ) ) ;
#4681 = EDGE_CURVE ( 'NONE', #3721, #760, #1235, .T. ) ;
#4682 = DIRECTION ( 'NONE',  ( -1.000000000000000000, 0.000000000000000000, 0.000000000000000000 ) ) ;
#4683 = CARTESIAN_POINT ( 'NONE',  ( -7.301858691287086423, -3.172613069824385068, 1.999999999999998224 ) ) ;
#4684 = DIRECTION ( 'NONE',  ( -0.000000000000000000, -0.000000000000000000, -1.000000000000000000 ) ) ;
#4685 = CARTESIAN_POINT ( 'NONE',  ( 6.824478893064963358, -1.828844244265460217, 13.99999999999999645 ) ) ;
#4686 = EDGE_CURVE ( 'NONE', #1983, #4504, #3255, .T. ) ;
#4687 = CARTESIAN_POINT ( 'NONE',  ( -9.273719170356997665, -3.669762015052091098, 1.999999999999998224 ) ) ;
#4688 = DIRECTION ( 'NONE',  ( 0.000000000000000000, 0.000000000000000000, -1.000000000000000000 ) ) ;
#4689 = DIRECTION ( 'NONE',  ( -1.000000000000000000, 0.000000000000000000, 0.000000000000000000 ) ) ;
#4690 = ORIENTED_EDGE ( 'NONE', *, *, #5077, .T. ) ;
#4691 = PLANE ( 'NONE',  #5211 ) ;
#4692 = DIRECTION ( 'NONE',  ( 0.000000000000000000, 0.000000000000000000, -1.000000000000000000 ) ) ;
#4693 = CARTESIAN_POINT ( 'NONE',  ( -9.533152408061617678, 0.1566715252477025866, 1.999999999999998224 ) ) ;
#4694 = CARTESIAN_POINT ( 'NONE',  ( 5.862282306371745300, 6.688714470717012972, 13.99999999999999645 ) ) ;
#4695 = DIRECTION ( 'NONE',  ( -1.000000000000000000, 0.000000000000000000, 0.000000000000000000 ) ) ;
#4696 = EDGE_CURVE ( 'NONE', #2946, #4270, #3625, .T. ) ;
#4697 = VERTEX_POINT ( 'NONE', #3070 ) ;
#4698 = CARTESIAN_POINT ( 'NONE',  ( 0.000000000000000000, 0.000000000000000000, 0.000000000000000000 ) ) ;
#4699 = ORIENTED_EDGE ( 'NONE', *, *, #4224, .F. ) ;
#4700 = DIRECTION ( 'NONE',  ( -4.364351673553916694E-15, 1.000000000000000000, 0.000000000000000000 ) ) ;
#4701 = CARTESIAN_POINT ( 'NONE',  ( 2.369394374793903246, -7.353877281245580377, 14.00000000000000000 ) ) ;
#4702 = CARTESIAN_POINT ( 'NONE',  ( 7.456063200421762183, 7.959410280422752670, 13.99999999999999645 ) ) ;
#4703 = CARTESIAN_POINT ( 'NONE',  ( 7.280083392764700179, -2.072676875633882254, 14.00000000000000000 ) ) ;
#4704 = ORIENTED_EDGE ( 'NONE', *, *, #364, .T. ) ;
#4705 = CARTESIAN_POINT ( 'NONE',  ( 7.066195124645999748, -7.302433507960749637, 1.999999999999998224 ) ) ;
#4706 = FACE_OUTER_BOUND ( 'NONE', #3093, .T. ) ;
#4707 = CARTESIAN_POINT ( 'NONE',  ( 0.000000000000000000, 0.000000000000000000, 15.10000000000000142 ) ) ;
#4708 = CARTESIAN_POINT ( 'NONE',  ( -6.826495404309643966, 4.393449859560456083, 1.999999999999998224 ) ) ;
#4709 = CARTESIAN_POINT ( 'NONE',  ( -6.112420884766618379, -2.295018720694776526, 1.999999999999998224 ) ) ;
#4710 = CARTESIAN_POINT ( 'NONE',  ( 5.213743241621229707, -4.883528188333805531, 13.99999999999999645 ) ) ;
#4711 = FILL_AREA_STYLE_COLOUR ( '', #1792 ) ;
#4712 = CARTESIAN_POINT ( 'NONE',  ( 1.511842404626676961, 9.183516746439465805, 1.999999999999998224 ) ) ;
#4713 = DIRECTION ( 'NONE',  ( -1.000000000000000000, -0.000000000000000000, -0.000000000000000000 ) ) ;
#4714 = AXIS2_PLACEMENT_3D ( 'NONE', #2702, #3914, #5668 ) ;
#4715 = CARTESIAN_POINT ( 'NONE',  ( -15.00000000000000000, 0.000000000000000000, 12.00000000000000000 ) ) ;
#4716 = ORIENTED_EDGE ( 'NONE', *, *, #4407, .F. ) ;
#4717 = FACE_OUTER_BOUND ( 'NONE', #3655, .T. ) ;
#4718 = DIRECTION ( 'NONE',  ( -0.000000000000000000, 0.5000000000000001110, 0.8660254037844385966 ) ) ;
#4719 = AXIS2_PLACEMENT_3D ( 'NONE', #523, #1010, #2303 ) ;
#4720 = CARTESIAN_POINT ( 'NONE',  ( -1.063411474431080528, -9.238278818535565762, 13.99999999999999645 ) ) ;
#4721 = DIRECTION ( 'NONE',  ( -0.000000000000000000, -0.000000000000000000, 1.000000000000000000 ) ) ;
#4722 = EDGE_LOOP ( 'NONE', ( #3376, #2820 ) ) ;
#4723 = LINE ( 'NONE', #5251, #1156 ) ;
#4724 = ORIENTED_EDGE ( 'NONE', *, *, #3592, .T. ) ;
#4725 = CARTESIAN_POINT ( 'NONE',  ( 0.000000000000000000, 0.000000000000000000, 2.000000000000000000 ) ) ;
#4726 = AXIS2_PLACEMENT_3D ( 'NONE', #1085, #2847, #107 ) ;
#4727 = CARTESIAN_POINT ( 'NONE',  ( 4.415008247871436531, 7.106745273741267965, 14.00000000000000000 ) ) ;
#4728 = CARTESIAN_POINT ( 'NONE',  ( -2.965071238690785371, 6.007415411094349622, 1.999999999999998224 ) ) ;
#4729 = AXIS2_PLACEMENT_3D ( 'NONE', #1404, #3457, #374 ) ;
#4730 = CARTESIAN_POINT ( 'NONE',  ( -5.000000000000085265, 24.49489742783176638, -8.000000000000000000 ) ) ;
#4731 = CARTESIAN_POINT ( 'NONE',  ( -2.189112655477411185, -6.464091385745795115, 14.00000000000000000 ) ) ;
#4732 = VERTEX_POINT ( 'NONE', #2982 ) ;
#4733 = CARTESIAN_POINT ( 'NONE',  ( 9.650319724628623419, 2.588775111615904567, 1.999999999999998224 ) ) ;
#4734 = AXIS2_PLACEMENT_3D ( 'NONE', #3893, #1654, #5618 ) ;
#4735 = CARTESIAN_POINT ( 'NONE',  ( 0.000000000000000000, 0.000000000000000000, 12.00000000000000000 ) ) ;
#4736 = CARTESIAN_POINT ( 'NONE',  ( 0.000000000000000000, 0.000000000000000000, 0.000000000000000000 ) ) ;
#4737 = CARTESIAN_POINT ( 'NONE',  ( 8.518575158373787204, 0.2826087140540892162, 1.999999999999998224 ) ) ;
#4738 = VECTOR ( 'NONE', #2041, 1000.000000000000000 ) ;
#4739 = CARTESIAN_POINT ( 'NONE',  ( -5.432680616545222385, 3.899654942179428652, 2.000000000001176392 ) ) ;
#4740 = CARTESIAN_POINT ( 'NONE',  ( 5.194219494279654015, 4.554949839096549269, 13.99999999999999645 ) ) ;
#4741 = AXIS2_PLACEMENT_3D ( 'NONE', #5612, #1673, #5181 ) ;
#4742 = SURFACE_STYLE_USAGE ( .BOTH. , #1210 ) ;
#4743 = CARTESIAN_POINT ( 'NONE',  ( -0.6809175113353352904, 10.25113960786383771, 1.999999999999998224 ) ) ;
#4744 = VECTOR ( 'NONE', #3694, 1000.000000000000000 ) ;
#4745 = CYLINDRICAL_SURFACE ( 'NONE', #5295, 23.00000000000000000 ) ;
#4746 = PLANE ( 'NONE',  #2996 ) ;
#4747 = ORIENTED_EDGE ( 'NONE', *, *, #4606, .F. ) ;
#4748 = PLANE ( 'NONE',  #3099 ) ;
#4749 = LINE ( 'NONE', #5220, #2067 ) ;
#4750 = CIRCLE ( 'NONE', #68, 23.00000000000000000 ) ;
#4751 = CARTESIAN_POINT ( 'NONE',  ( -6.537688394901546296, -6.759197365499824528, 13.99999999999999645 ) ) ;
#4752 = FACE_OUTER_BOUND ( 'NONE', #5480, .T. ) ;
#4753 = ORIENTED_EDGE ( 'NONE', *, *, #4696, .F. ) ;
#4754 = CARTESIAN_POINT ( 'NONE',  ( -5.000000000000085265, 24.49489742783176638, 8.000000000000000000 ) ) ;
#4755 = VERTEX_POINT ( 'NONE', #4730 ) ;
#4756 = AXIS2_PLACEMENT_3D ( 'NONE', #473, #5234, #5260 ) ;
#4757 = DIRECTION ( 'NONE',  ( 0.000000000000000000, 0.000000000000000000, -1.000000000000000000 ) ) ;
#4758 = CARTESIAN_POINT ( 'NONE',  ( 7.990059919442007441, -3.149571442993018167, 14.00000000000000000 ) ) ;
#4759 = EDGE_CURVE ( 'NONE', #354, #3849, #3349, .T. ) ;
#4760 = CARTESIAN_POINT ( 'NONE',  ( -10.26372689808646577, -2.219791875069885290, 13.99999999999999645 ) ) ;
#4761 = PRODUCT_DEFINITION_CONTEXT ( 'detailed design', #1809, 'design' ) ;
#4762 = CARTESIAN_POINT ( 'NONE',  ( 1.300000000000000044, 0.7216878364870328300, -1.250000000000000000 ) ) ;
#4763 = CARTESIAN_POINT ( 'NONE',  ( 4.064490656458173312, -6.524520197619847472, 14.00000000000000000 ) ) ;
#4764 = VERTEX_POINT ( 'NONE', #5624 ) ;
#4765 = CARTESIAN_POINT ( 'NONE',  ( 6.769338797470902946, 8.534199679356609280, 1.999999999999998224 ) ) ;
#4766 = EDGE_CURVE ( 'NONE', #586, #4732, #5553, .T. ) ;
#4767 = CARTESIAN_POINT ( 'NONE',  ( 0.5931392160223177834, -7.236979168992432321, 13.99999999999999645 ) ) ;
#4768 = CONTEXT_DEPENDENT_SHAPE_REPRESENTATION ( #4166, #4271 ) ;
#4769 = CARTESIAN_POINT ( 'NONE',  ( 8.256732931686219246, 4.597988481711511533, 1.999999999999998224 ) ) ;
#4770 = ADVANCED_FACE ( 'NONE', ( #1742 ), #3989, .F. ) ;
#4771 = CARTESIAN_POINT ( 'NONE',  ( -0.2539011084975961174, 7.766605221862830533, 1.999999999999998224 ) ) ;
#4772 = CARTESIAN_POINT ( 'NONE',  ( -2.263950162103714359, 8.438937471999240714, 13.99999999999999645 ) ) ;
#4773 = DIRECTION ( 'NONE',  ( 0.000000000000000000, 0.000000000000000000, -1.000000000000000000 ) ) ;
#4774 = CARTESIAN_POINT ( 'NONE',  ( 5.071900148311750733, 7.881338450276374807, 1.999999999999998224 ) ) ;
#4775 = DIRECTION ( 'NONE',  ( -1.000000000000000000, 0.000000000000000000, 0.000000000000000000 ) ) ;
#4776 = FILL_AREA_STYLE ('',( #5556 ) ) ;
#4777 = ORIENTED_EDGE ( 'NONE', *, *, #3010, .F. ) ;
#4778 = CARTESIAN_POINT ( 'NONE',  ( 13.00000000000000178, 0.000000000000000000, 4.000000000000003553 ) ) ;
#4779 = CARTESIAN_POINT ( 'NONE',  ( 8.973806924230895987, -1.178693538871703250, 13.99999999999999645 ) ) ;
#4780 = PRODUCT_DEFINITION ( 'UNKNOWN', '', #389, #793 ) ;
#4781 = CARTESIAN_POINT ( 'NONE',  ( 2.199999999999999289, 0.000000000000000000, -3.100000000000000533 ) ) ;
#4782 = ORIENTED_EDGE ( 'NONE', *, *, #2389, .T. ) ;
#4783 = CARTESIAN_POINT ( 'NONE',  ( 10.20000000000000107, 0.000000000000000000, 0.000000000000000000 ) ) ;
#4784 = ORIENTED_EDGE ( 'NONE', *, *, #4431, .F. ) ;
#4785 = LINE ( 'NONE', #2171, #5669 ) ;
#4786 = CARTESIAN_POINT ( 'NONE',  ( 6.929006764466010715, 4.804313515625074693, 14.00000000000000000 ) ) ;
#4787 = CARTESIAN_POINT ( 'NONE',  ( 11.00000000000000355, -2.488243985854232676E-14, 13.99999999999999645 ) ) ;
#4788 = DIRECTION ( 'NONE',  ( -1.000000000000000000, -8.881784197001250746E-15, 0.000000000000000000 ) ) ;
#4789 = CARTESIAN_POINT ( 'NONE',  ( 8.518575158374426692, 0.2826087140540691767, 14.00000000000000000 ) ) ;
#4790 = EDGE_CURVE ( 'NONE', #1000, #1733, #5374, .T. ) ;
#4791 = ORIENTED_EDGE ( 'NONE', *, *, #2567, .F. ) ;
#4792 = DIRECTION ( 'NONE',  ( 1.000000000000000000, 0.000000000000000000, 0.000000000000000000 ) ) ;
#4793 = CARTESIAN_POINT ( 'NONE',  ( 1.183015137239217696, -7.150809911821260911, 13.99999999999999645 ) ) ;
#4794 = APPLICATION_PROTOCOL_DEFINITION ( 'draft international standard', 'automotive_design', 1998, #894 ) ;
#4795 = CARTESIAN_POINT ( 'NONE',  ( 2.992331685656917539, 8.840389773664522721, 1.999999999999998224 ) ) ;
#4796 = CARTESIAN_POINT ( 'NONE',  ( 5.213743241621227931, -4.883528188333804643, 1.999999999999998224 ) ) ;
#4797 = CARTESIAN_POINT ( 'NONE',  ( 5.862282306371745300, 6.688714470717012972, 13.99999999999999645 ) ) ;
#4798 = DIRECTION ( 'NONE',  ( 1.000000000000000000, 0.000000000000000000, -0.000000000000000000 ) ) ;
#4799 = DIRECTION ( 'NONE',  ( 0.9981983770774224274, -0.06000000000000008105, 0.000000000000000000 ) ) ;
#4800 = DIRECTION ( 'NONE',  ( -1.000000000000000000, 0.000000000000000000, 0.000000000000000000 ) ) ;
#4801 = FACE_OUTER_BOUND ( 'NONE', #2591, .T. ) ;
#4802 = VERTEX_POINT ( 'NONE', #4415 ) ;
#4803 = DIRECTION ( 'NONE',  ( 1.000000000000000000, 0.000000000000000000, 0.000000000000000000 ) ) ;
#4804 = CARTESIAN_POINT ( 'NONE',  ( -10.26372689808646577, -2.219791875069885290, 13.99999999999999645 ) ) ;
#4805 = VECTOR ( 'NONE', #1706, 1000.000000000000000 ) ;
#4806 =( NAMED_UNIT ( * ) PLANE_ANGLE_UNIT ( ) SI_UNIT ( $, .RADIAN. ) );
#4807 = ORIENTED_EDGE ( 'NONE', *, *, #3739, .F. ) ;
#4808 = FACE_BOUND ( 'NONE', #2405, .T. ) ;
#4809 = ORIENTED_EDGE ( 'NONE', *, *, #1864, .T. ) ;
#4810 = ORIENTED_EDGE ( 'NONE', *, *, #4657, .T. ) ;
#4811 = CARTESIAN_POINT ( 'NONE',  ( -0.1423371034015828429, 8.273642750286580139, 14.00000000000000000 ) ) ;
#4812 = CARTESIAN_POINT ( 'NONE',  ( 1.623707939105925702, -6.078451570951504124, 1.999999999999998224 ) ) ;
#4813 = EDGE_CURVE ( 'NONE', #4349, #4241, #3804, .T. ) ;
#4814 = AXIS2_PLACEMENT_3D ( 'NONE', #5469, #2548, #847 ) ;
#4815 = FACE_OUTER_BOUND ( 'NONE', #1708, .T. ) ;
#4816 = CARTESIAN_POINT ( 'NONE',  ( 6.592258996018688144, -3.799026305082323418, 14.00000000000000000 ) ) ;
#4817 = VECTOR ( 'NONE', #2609, 1000.000000000000000 ) ;
#4818 = ORIENTED_EDGE ( 'NONE', *, *, #2118, .F. ) ;
#4819 = DIRECTION ( 'NONE',  ( 0.000000000000000000, 0.000000000000000000, 1.000000000000000000 ) ) ;
#4820 = CIRCLE ( 'NONE', #2621, 22.50000000000000355 ) ;
#4821 = PRESENTATION_LAYER_ASSIGNMENT (  '', '', ( #1610 ) ) ;
#4822 = CARTESIAN_POINT ( 'NONE',  ( -2.466819000628047487, 6.242838961510106977, 13.99999999999999645 ) ) ;
#4823 = APPLICATION_PROTOCOL_DEFINITION ( 'draft international standard', 'automotive_design', 1998, #822 ) ;
#4824 = CARTESIAN_POINT ( 'NONE',  ( 6.863489721961431478, 6.439594285167053123, 1.999999999999998224 ) ) ;
#4825 = ADVANCED_FACE ( 'NONE', ( #4815 ), #1288, .T. ) ;
#4826 = CARTESIAN_POINT ( 'NONE',  ( 0.5931392160223177834, -7.236979168992430544, 1.999999999999998224 ) ) ;
#4827 = ADVANCED_FACE ( 'NONE', ( #878 ), #2637, .T. ) ;
#4828 = DIRECTION ( 'NONE',  ( -1.000000000000000000, 0.000000000000000000, 0.000000000000000000 ) ) ;
#4829 = VECTOR ( 'NONE', #2909, 1000.000000000000114 ) ;
#4830 =( LENGTH_UNIT ( ) NAMED_UNIT ( * ) SI_UNIT ( .MILLI., .METRE. ) );
#4831 = CARTESIAN_POINT ( 'NONE',  ( 2.400000000000000799, 0.000000000000000000, 0.000000000000000000 ) ) ;
#4832 = ADVANCED_FACE ( 'NONE', ( #15, #3522 ), #3083, .T. ) ;
#4833 = CARTESIAN_POINT ( 'NONE',  ( -2.283612537812033771, 5.775797914528922661, 1.999999999999998224 ) ) ;
#4834 = CARTESIAN_POINT ( 'NONE',  ( 0.000000000000000000, 0.000000000000000000, 12.00000000000000000 ) ) ;
#4835 = ORIENTED_EDGE ( 'NONE', *, *, #2442, .T. ) ;
#4836 = CIRCLE ( 'NONE', #5574, 3.799999999999999378 ) ;
#4837 = DIRECTION ( 'NONE',  ( 1.000000000000000000, 0.000000000000000000, 0.000000000000000000 ) ) ;
#4838 = CARTESIAN_POINT ( 'NONE',  ( 9.807503887221459493, -2.283819133639753751, 13.99999999999999645 ) ) ;
#4839 = CIRCLE ( 'NONE', #1989, 0.2500000000000002220 ) ;
#4840 = ORIENTED_EDGE ( 'NONE', *, *, #2965, .F. ) ;
#4841 = CARTESIAN_POINT ( 'NONE',  ( 22.50000000000000355, 2.755455298081545172E-15, 14.00000000000000000 ) ) ;
#4842 = VERTEX_POINT ( 'NONE', #4861 ) ;
#4843 = ADVANCED_FACE ( 'NONE', ( #944 ), #3139, .F. ) ;
#4844 = VERTEX_POINT ( 'NONE', #2617 ) ;
#4845 = CARTESIAN_POINT ( 'NONE',  ( -7.425829140954380847, 3.215541426300493111, 14.00000000000000000 ) ) ;
#4846 = CARTESIAN_POINT ( 'NONE',  ( -4.372214883940050534, 6.312905667202751481, 1.999999999999998224 ) ) ;
#4847 = AXIS2_PLACEMENT_3D ( 'NONE', #215, #1969, #4592 ) ;
#4848 = CARTESIAN_POINT ( 'NONE',  ( 6.000000000000000888, 0.000000000000000000, 7.999999999999996447 ) ) ;
#4849 = CARTESIAN_POINT ( 'NONE',  ( 3.208073253695060245, -8.107602109809697311, 14.00000000000000000 ) ) ;
#4850 = VECTOR ( 'NONE', #4031, 1000.000000000000000 ) ;
#4851 = VERTEX_POINT ( 'NONE', #2214 ) ;
#4852 = CARTESIAN_POINT ( 'NONE',  ( -3.867583043141952892, 8.914321633328466277, 1.999999999999998224 ) ) ;
#4853 = CARTESIAN_POINT ( 'NONE',  ( -8.741731599017841248, 6.051300285686449953, 1.999999999999998224 ) ) ;
#4854 = SHAPE_REPRESENTATION ( 'TAS-001', ( #5359, #4529, #3428, #5447, #4255, #573, #1407, #2045 ), #4436 ) ;
#4855 = CARTESIAN_POINT ( 'NONE',  ( -6.112420884766619267, -2.295018720694776970, 13.99999999999999645 ) ) ;
#4856 = CONTEXT_DEPENDENT_SHAPE_REPRESENTATION ( #2396, #3490 ) ;
#4857 = CARTESIAN_POINT ( 'NONE',  ( 6.721134410589269415, -6.938257756003234356, 1.999999999999998224 ) ) ;
#4858 = PRODUCT_DEFINITION ( 'UNKNOWN', '', #298, #4308 ) ;
#4859 = CARTESIAN_POINT ( 'NONE',  ( -6.505530684480364201, -3.618119970335912150, 1.999999999999998224 ) ) ;
#4860 = LINE ( 'NONE', #943, #4372 ) ;
#4861 = CARTESIAN_POINT ( 'NONE',  ( 1.380000000000002558, 21.95856267278071527, 12.00000000000000000 ) ) ;
#4862 = CARTESIAN_POINT ( 'NONE',  ( 0.000000000000000000, 0.000000000000000000, 4.000000000000003553 ) ) ;
#4863 = CARTESIAN_POINT ( 'NONE',  ( 6.160418207306092242, 1.983851483784910164, 1.999999999999998224 ) ) ;
#4864 = CYLINDRICAL_SURFACE ( 'NONE', #2366, 4.500000000000000888 ) ;
#4865 = ORIENTED_EDGE ( 'NONE', *, *, #2379, .F. ) ;
#4866 = SURFACE_STYLE_USAGE ( .BOTH. , #3119 ) ;
#4867 = EDGE_CURVE ( 'NONE', #4764, #3158, #685, .T. ) ;
#4868 = DIRECTION ( 'NONE',  ( -1.000000000000000000, 0.000000000000000000, 0.000000000000000000 ) ) ;
#4869 = FILL_AREA_STYLE_COLOUR ( '', #5282 ) ;
#4870 = CYLINDRICAL_SURFACE ( 'NONE', #886, 12.50000000000000000 ) ;
#4871 = ORIENTED_EDGE ( 'NONE', *, *, #687, .F. ) ;
#4872 = VERTEX_POINT ( 'NONE', #917 ) ;
#4873 = CARTESIAN_POINT ( 'NONE',  ( -1.271096247112511346, -9.720655361064800104, 14.00000000000000000 ) ) ;
#4874 = CARTESIAN_POINT ( 'NONE',  ( -0.5931392160223127874, -7.263020831007572120, 1.999999999999998224 ) ) ;
#4875 = ADVANCED_FACE ( 'NONE', ( #3965 ), #1693, .F. ) ;
#4876 = CARTESIAN_POINT ( 'NONE',  ( 7.311638624438941747, 4.225618826270679307, 1.999999999999998224 ) ) ;
#4877 = CARTESIAN_POINT ( 'NONE',  ( -7.550296695602809471, -2.566425989403007257, 14.00000000000000000 ) ) ;
#4878 = ORIENTED_EDGE ( 'NONE', *, *, #2535, .F. ) ;
#4879 = CARTESIAN_POINT ( 'NONE',  ( -2.179108132477198367, -10.08557389312680108, 1.999999999999998224 ) ) ;
#4880 = CYLINDRICAL_SURFACE ( 'NONE', #3565, 22.50000000000000355 ) ;
#4881 = CARTESIAN_POINT ( 'NONE',  ( -1.451466707715608040, -6.203196315423898710, 13.99999999999999645 ) ) ;
#4882 = CONTEXT_DEPENDENT_SHAPE_REPRESENTATION ( #2990, #1092 ) ;
#4883 = CARTESIAN_POINT ( 'NONE',  ( -7.963215149404742732, -4.094909132697305054, 1.999999999999998224 ) ) ;
#4884 = CARTESIAN_POINT ( 'NONE',  ( -5.322107489685658166, 5.499660323246576610, 1.999999999999998224 ) ) ;
#4885 = LINE ( 'NONE', #513, #4092 ) ;
#4886 = DIRECTION ( 'NONE',  ( 1.000000000000000000, 0.000000000000000000, 0.000000000000000000 ) ) ;
#4887 = PRESENTATION_STYLE_ASSIGNMENT (( #1729 ) ) ;
#4888 = CARTESIAN_POINT ( 'NONE',  ( -3.922355934210176809, -4.464780306276820099, 1.999999999999998224 ) ) ;
#4889 = CARTESIAN_POINT ( 'NONE',  ( -1.380000000000002558, 21.95856267278071527, 4.000000000000000000 ) ) ;
#4890 = CARTESIAN_POINT ( 'NONE',  ( 0.000000000000000000, 0.000000000000000000, -3.100000000000000533 ) ) ;
#4891 = ORIENTED_EDGE ( 'NONE', *, *, #4344, .T. ) ;
#4892 = DIRECTION ( 'NONE',  ( 0.000000000000000000, 0.000000000000000000, 1.000000000000000000 ) ) ;
#4893 = MECHANICAL_DESIGN_GEOMETRIC_PRESENTATION_REPRESENTATION (  '', ( #1610 ), #2410 ) ;
#4894 = CARTESIAN_POINT ( 'NONE',  ( -5.000000000000085265, 24.49489742783176638, -5.000000000000000000 ) ) ;
#4895 = DIRECTION ( 'NONE',  ( -1.000000000000000000, 3.540989467475305966E-16, 0.000000000000000000 ) ) ;
#4896 = CARTESIAN_POINT ( 'NONE',  ( 18.00000000000000000, 1.553654299240552096E-15, 8.000000000000000000 ) ) ;
#4897 = ORIENTED_EDGE ( 'NONE', *, *, #1211, .T. ) ;
#4898 = LINE ( 'NONE', #957, #612 ) ;
#4899 = CARTESIAN_POINT ( 'NONE',  ( -9.926332099419621358, -1.311590842189569894, 14.00000000000000000 ) ) ;
#4900 = CARTESIAN_POINT ( 'NONE',  ( -2.721086536275891810, 7.222755814214461445, 1.999999999999998224 ) ) ;
#4901 = CARTESIAN_POINT ( 'NONE',  ( 3.208073253695059801, -8.107602109809695534, 1.999999999999998224 ) ) ;
#4902 = EDGE_CURVE ( 'NONE', #1326, #726, #2674, .T. ) ;
#4903 = CARTESIAN_POINT ( 'NONE',  ( 6.721134410589271191, -6.938257756002876420, 14.00000000000000000 ) ) ;
#4904 = ORIENTED_EDGE ( 'NONE', *, *, #1927, .T. ) ;
#4905 = CARTESIAN_POINT ( 'NONE',  ( -9.197478219253614640, 5.306711421960435437, 1.999999999999998224 ) ) ;
#4906 = AXIS2_PLACEMENT_3D ( 'NONE', #4831, #5688, #2189 ) ;
#4907 = LINE ( 'NONE', #1916, #2834 ) ;
#4908 = CARTESIAN_POINT ( 'NONE',  ( 2.519353604429575011, -7.832629354751150963, 13.99999999999999645 ) ) ;
#4909 = CARTESIAN_POINT ( 'NONE',  ( 7.024953159363689359, -4.052930060063556716, 13.99999999999999645 ) ) ;
#4910 = AXIS2_PLACEMENT_3D ( 'NONE', #3709, #5007, #1065 ) ;
#4911 = CONTEXT_DEPENDENT_SHAPE_REPRESENTATION ( #3069, #1141 ) ;
#4912 = CARTESIAN_POINT ( 'NONE',  ( -9.692812185270616610, 2.758747493781260829, 1.999999999999998224 ) ) ;
#4913 = CARTESIAN_POINT ( 'NONE',  ( 6.679452517770526399, -4.623421500472435497, 1.999999999999998224 ) ) ;
#4914 = LINE ( 'NONE', #4027, #1703 ) ;
#4915 = CIRCLE ( 'NONE', #3533, 22.50000000000000355 ) ;
#4916 = CARTESIAN_POINT ( 'NONE',  ( -1.379999999999999893, 22.95856267278071172, 5.000000000000000888 ) ) ;
#4917 = CARTESIAN_POINT ( 'NONE',  ( 17.99999999999999289, -15.01665741768121443, -8.000000000000000000 ) ) ;
#4918 = AXIS2_PLACEMENT_3D ( 'NONE', #2534, #813, #3429 ) ;
#4919 = CARTESIAN_POINT ( 'NONE',  ( 0.7175617537426045578, 6.248173425771537559, 1.999999999999998224 ) ) ;
#4920 = CARTESIAN_POINT ( 'NONE',  ( 2.000000000000000000, 0.000000000000000000, 4.000000000000000000 ) ) ;
#4921 = VECTOR ( 'NONE', #5510, 1000.000000000000000 ) ;
#4922 = CARTESIAN_POINT ( 'NONE',  ( 10.02932042447482353, 0.1670047327946668492, 13.99999999999999645 ) ) ;
#4923 = CARTESIAN_POINT ( 'NONE',  ( 0.000000000000000000, 0.000000000000000000, 8.000000000000000000 ) ) ;
#4924 = EDGE_CURVE ( 'NONE', #4096, #525, #2156, .T. ) ;
#4925 = VECTOR ( 'NONE', #5609, 1000.000000000000000 ) ;
#4926 = CARTESIAN_POINT ( 'NONE',  ( 22.50000000000000355, 2.755455298081545172E-15, 12.00000000000000000 ) ) ;
#4927 = ORIENTED_EDGE ( 'NONE', *, *, #3014, .T. ) ;
#4928 = ORIENTED_EDGE ( 'NONE', *, *, #190, .F. ) ;
#4929 = CARTESIAN_POINT ( 'NONE',  ( 3.433597602020987072, -9.098706718024024198, 14.00000000000000000 ) ) ;
#4930 = CARTESIAN_POINT ( 'NONE',  ( 0.5931392160223177834, -7.236979168992430544, 1.999999999999998224 ) ) ;
#4931=STYLED_ITEM('',(#5737),#652);
#4932 = CARTESIAN_POINT ( 'NONE',  ( 5.528193227148988420, 6.314447692498917242, 1.999999999999998224 ) ) ;
#4933 = CARTESIAN_POINT ( 'NONE',  ( -5.048038583874033591, -7.300734008993382318, 14.00000000000000000 ) ) ;
#4934 = EDGE_CURVE ( 'NONE', #3623, #2844, #25, .T. ) ;
#4935 = ORIENTED_EDGE ( 'NONE', *, *, #5183, .T. ) ;
#4936 = TOROIDAL_SURFACE ( 'NONE', #3651, 2.199999999999999289, 0.2000000000000000111 ) ;
#4937 = CARTESIAN_POINT ( 'NONE',  ( -7.044187934146015628, 6.598551529631267343, 1.999999999999998224 ) ) ;
#4938 = CARTESIAN_POINT ( 'NONE',  ( 4.999999999999914735, 24.49489742783179835, -5.000000000000000000 ) ) ;
#4939 = CARTESIAN_POINT ( 'NONE',  ( -2.153669193480074018, -8.035861145135083206, 13.99999999999999645 ) ) ;
#4940 = CARTESIAN_POINT ( 'NONE',  ( -5.741039858921713979, -6.128965587877692300, 13.99999999999999645 ) ) ;
#4941 = CARTESIAN_POINT ( 'NONE',  ( 5.030817567586499450, 9.062633982223127660, 1.999999999999998224 ) ) ;
#4942 = ORIENTED_EDGE ( 'NONE', *, *, #5126, .F. ) ;
#4943 = CARTESIAN_POINT ( 'NONE',  ( 6.401046915551857452, 6.194151307162986342, 1.999999999999998224 ) ) ;
#4944 = DIRECTION ( 'NONE',  ( -1.000000000000000000, 0.000000000000000000, 0.000000000000000000 ) ) ;
#4945 = CARTESIAN_POINT ( 'NONE',  ( 5.500000000000001776, 0.000000000000000000, 14.00000000000000000 ) ) ;
#4946 = CARTESIAN_POINT ( 'NONE',  ( 5.733165789232423037, 2.946509839760266924, 1.999999999999998224 ) ) ;
#4947 = EDGE_CURVE ( 'NONE', #3623, #300, #3113, .T. ) ;
#4948 = ORIENTED_EDGE ( 'NONE', *, *, #3567, .F. ) ;
#4949 = CARTESIAN_POINT ( 'NONE',  ( 4.290186206382708534, 5.996800006796977556, 1.999999999999998224 ) ) ;
#4950 = CARTESIAN_POINT ( 'NONE',  ( 23.24999999999999645, -8.485281374238580199, 4.000000000000000000 ) ) ;
#4951 = PRESENTATION_STYLE_ASSIGNMENT (( #3253 ) ) ;
#4952 = CARTESIAN_POINT ( 'NONE',  ( 21.99999999999999645, -30.00000000000000000, 12.00000000000000000 ) ) ;
#4953 =( NAMED_UNIT ( * ) PLANE_ANGLE_UNIT ( ) SI_UNIT ( $, .RADIAN. ) );
#4954 = CYLINDRICAL_SURFACE ( 'NONE', #3449, 5.000000000000000000 ) ;
#4955 = ORIENTED_EDGE ( 'NONE', *, *, #3022, .T. ) ;
#4956 = FACE_OUTER_BOUND ( 'NONE', #5098, .T. ) ;
#4957 = CARTESIAN_POINT ( 'NONE',  ( -9.273719170356997665, -3.669762015051720727, 14.00000000000000000 ) ) ;
#4958 = CARTESIAN_POINT ( 'NONE',  ( 6.033242055734851839, 5.122103984031729063, 1.999999999999998224 ) ) ;
#4959 = CARTESIAN_POINT ( 'NONE',  ( -6.700137237869126849, -5.881230172875862472, 1.999999999999998224 ) ) ;
#4960 = CARTESIAN_POINT ( 'NONE',  ( 3.713512749563263604, 8.576920285551967282, 14.00000000000000000 ) ) ;
#4961 = ORIENTED_EDGE ( 'NONE', *, *, #1114, .F. ) ;
#4962 = CARTESIAN_POINT ( 'NONE',  ( 9.599547022228483328, -3.085197981542975310, 1.999999999999998224 ) ) ;
#4963 = CARTESIAN_POINT ( 'NONE',  ( -2.744490807750914918, 5.556819979548927257, 14.00000000000000000 ) ) ;
#4964 = CARTESIAN_POINT ( 'NONE',  ( 7.409328306158469601, 2.927536720054149555, 13.99999999999999645 ) ) ;
#4965 = CARTESIAN_POINT ( 'NONE',  ( -10.03347820201762630, 0.3196629254998830660, 1.999999999999998224 ) ) ;
#4966 = EDGE_LOOP ( 'NONE', ( #2331, #1273, #1919, #2103 ) ) ;
#4967 = CARTESIAN_POINT ( 'NONE',  ( 5.933674912743041041, -6.989438080420770305, 1.999999999999998224 ) ) ;
#4968 = LINE ( 'NONE', #2784, #1696 ) ;
#4969 = CARTESIAN_POINT ( 'NONE',  ( -0.8169484412210608060, 6.196426872864403634, 1.999999999999998224 ) ) ;
#4970 = ORIENTED_EDGE ( 'NONE', *, *, #3090, .T. ) ;
#4971 = CARTESIAN_POINT ( 'NONE',  ( -0.2403693791186040096, 7.265099133626553574, 1.999999999999998224 ) ) ;
#4972 = LINE ( 'NONE', #111, #5584 ) ;
#4973 = CARTESIAN_POINT ( 'NONE',  ( -1.379999999999999893, 22.95856267278071172, 4.000000000000000000 ) ) ;
#4974 = CARTESIAN_POINT ( 'NONE',  ( 3.885274725274726393, -8.673617379884035472E-16, 0.000000000000000000 ) ) ;
#4975 = ORIENTED_EDGE ( 'NONE', *, *, #352, .T. ) ;
#4976 = CARTESIAN_POINT ( 'NONE',  ( 0.000000000000000000, 0.000000000000000000, 14.00000000000000000 ) ) ;
#4977 = STYLED_ITEM ( 'NONE', ( #2381 ), #5006 ) ;
#4978 = CARTESIAN_POINT ( 'NONE',  ( -3.609299841826104416, -9.156952235374472338, 14.00000000000000000 ) ) ;
#4979 = CARTESIAN_POINT ( 'NONE',  ( 2.519353604429720228, -7.832629354751149187, 1.999999999999998224 ) ) ;
#4980 = EDGE_CURVE ( 'NONE', #525, #1733, #1298, .T. ) ;
#4981 = CARTESIAN_POINT ( 'NONE',  ( -0.1423371034015438186, 8.273642750285960190, 1.999999999999998224 ) ) ;
#4982 = PRODUCT_DEFINITION_FORMATION_WITH_SPECIFIED_SOURCE ( 'ANY', '', #2062, .NOT_KNOWN. ) ;
#4983 = CARTESIAN_POINT ( 'NONE',  ( -9.692812185271368008, 2.758747493781260385, 14.00000000000000000 ) ) ;
#4984 = LINE ( 'NONE', #2371, #1339 ) ;
#4985 = ORIENTED_EDGE ( 'NONE', *, *, #5029, .F. ) ;
#4986 = CARTESIAN_POINT ( 'NONE',  ( 17.99999999999999289, -17.34935157289748631, -4.000000000000000000 ) ) ;
#4987 = CARTESIAN_POINT ( 'NONE',  ( 0.7175617537426050019, 6.248173425771539335, 14.00000000000000000 ) ) ;
#4988 = CARTESIAN_POINT ( 'NONE',  ( 2.810994617404221962, -9.846529629020569274, 13.99999999999999645 ) ) ;
#4989 = ADVANCED_FACE ( 'NONE', ( #1728, #1778 ), #5294, .F. ) ;
#4990 = CARTESIAN_POINT ( 'NONE',  ( -0.3669926094919908621, -5.824518274481599533, 14.00000000000000000 ) ) ;
#4991 = AXIS2_PLACEMENT_3D ( 'NONE', #4216, #4157, #1964 ) ;
#4992 = VERTEX_POINT ( 'NONE', #480 ) ;
#4993 = CARTESIAN_POINT ( 'NONE',  ( -7.763712483375481810, -3.368527140560798827, 1.999999999999998224 ) ) ;
#4994 = VECTOR ( 'NONE', #3256, 1000.000000000000000 ) ;
#4995 = EDGE_CURVE ( 'NONE', #4235, #4627, #1046, .T. ) ;
#4996 = CARTESIAN_POINT ( 'NONE',  ( 0.000000000000000000, 0.000000000000000000, 12.00000000000000000 ) ) ;
#4997 = CARTESIAN_POINT ( 'NONE',  ( -1.987635485262058133, 6.951293809708865012, 1.999999999999998224 ) ) ;
#4998 = ORIENTED_EDGE ( 'NONE', *, *, #1122, .T. ) ;
#4999 = CARTESIAN_POINT ( 'NONE',  ( -5.034899347481144538, -4.722558430572731503, 1.999999999999998224 ) ) ;
#5000 = VECTOR ( 'NONE', #4568, 1000.000000000000000 ) ;
#5001 = FACE_OUTER_BOUND ( 'NONE', #4357, .T. ) ;
#5002 = EDGE_CURVE ( 'NONE', #4235, #2034, #2649, .T. ) ;
#5003 = AXIS2_PLACEMENT_3D ( 'NONE', #3859, #3886, #5179 ) ;
#5004 = STYLED_ITEM ( 'NONE', ( #2476 ), #69 ) ;
#5005 = CARTESIAN_POINT ( 'NONE',  ( 0.000000000000000000, 0.000000000000000000, 12.00000000000000000 ) ) ;
#5006 = ADVANCED_BREP_SHAPE_REPRESENTATION ( '', ( #4482, #1336 ), #5538 ) ;
#5007 = DIRECTION ( 'NONE',  ( 0.000000000000000000, 0.000000000000000000, -1.000000000000000000 ) ) ;
#5008 = DIRECTION ( 'NONE',  ( -1.000000000000000000, 0.000000000000000000, 0.000000000000000000 ) ) ;
#5009 = VERTEX_POINT ( 'NONE', #82 ) ;
#5010 = AXIS2_PLACEMENT_3D ( 'NONE', #4409, #927, #35 ) ;
#5011 = FACE_OUTER_BOUND ( 'NONE', #1759, .T. ) ;
#5012 = CARTESIAN_POINT ( 'NONE',  ( 6.452733273991772656, 8.145031704320798482, 14.00000000000000000 ) ) ;
#5013 = CARTESIAN_POINT ( 'NONE',  ( -7.763712483375481810, -3.368527140560798827, 1.999999999999998224 ) ) ;
#5014 = VECTOR ( 'NONE', #2500, 1000.000000000000000 ) ;
#5015 = CARTESIAN_POINT ( 'NONE',  ( -9.986481889893736863, 1.144076113142370899, 1.999999999999998224 ) ) ;
#5016 = CARTESIAN_POINT ( 'NONE',  ( 9.348788865899230416, 1.705571004836294646, 14.00000000000000000 ) ) ;
#5017 = ADVANCED_FACE ( 'NONE', ( #1810 ), #2187, .T. ) ;
#5018 = CARTESIAN_POINT ( 'NONE',  ( 0.000000000000000000, 0.000000000000000000, 12.00000000000000000 ) ) ;
#5019 = ORIENTED_EDGE ( 'NONE', *, *, #4034, .F. ) ;
#5020 = CARTESIAN_POINT ( 'NONE',  ( 10.86297249782008123, 1.796588950249126349, 1.999999999999998224 ) ) ;
#5021 = DIRECTION ( 'NONE',  ( -1.000000000000000000, 0.000000000000000000, 0.000000000000000000 ) ) ;
#5022 = CARTESIAN_POINT ( 'NONE',  ( 1.208067634251009270, -9.180948453718622559, 13.99999999999999645 ) ) ;
#5023 = AXIS2_PLACEMENT_3D ( 'NONE', #3403, #404, #781 ) ;
#5024 = CARTESIAN_POINT ( 'NONE',  ( -3.595699629853522872, 5.016010494498949868, 14.00000000000000000 ) ) ;
#5025 = AXIS2_PLACEMENT_3D ( 'NONE', #2141, #2111, #4757 ) ;
#5026 = ORIENTED_EDGE ( 'NONE', *, *, #1667, .F. ) ;
#5027 = CARTESIAN_POINT ( 'NONE',  ( 0.5754137710878161061, 8.770917875152035137, 1.999999999999998224 ) ) ;
#5028 = CARTESIAN_POINT ( 'NONE',  ( 23.00000000000000000, -2.816687638038912352E-15, -2.000000000000000000 ) ) ;
#5029 = EDGE_CURVE ( 'NONE', #2459, #5617, #945, .T. ) ;
#5030 =( NAMED_UNIT ( * ) SI_UNIT ( $, .STERADIAN. ) SOLID_ANGLE_UNIT ( ) );
#5031 = CARTESIAN_POINT ( 'NONE',  ( 6.523553822664517554, -0.1051741892335503609, 1.999999999999998224 ) ) ;
#5032 = ORIENTED_EDGE ( 'NONE', *, *, #4790, .T. ) ;
#5033 = AXIS2_PLACEMENT_3D ( 'NONE', #3131, #1745, #4367 ) ;
#5034 = CARTESIAN_POINT ( 'NONE',  ( 6.592258996018686368, -3.799026305082465971, 1.999999999999998224 ) ) ;
#5035 = DIRECTION ( 'NONE',  ( -1.000000000000000000, 0.000000000000000000, 0.000000000000000000 ) ) ;
#5036 = LINE ( 'NONE', #1559, #4452 ) ;
#5037 = CARTESIAN_POINT ( 'NONE',  ( 9.809999999999998721, 0.000000000000000000, 0.000000000000000000 ) ) ;
#5038 = ORIENTED_EDGE ( 'NONE', *, *, #81, .F. ) ;
#5039 = CARTESIAN_POINT ( 'NONE',  ( 21.74999999999999645, -30.00000000000000000, 4.000000000000001776 ) ) ;
#5040 = CARTESIAN_POINT ( 'NONE',  ( 4.264126983937992499, 9.433107915010287670, 14.00000000000000000 ) ) ;
#5041 = CARTESIAN_POINT ( 'NONE',  ( 0.5432484998931219611, -8.249156888542632515, 1.999999999999998224 ) ) ;
#5042 = CARTESIAN_POINT ( 'NONE',  ( -6.681468852107525613, -5.130140014479350974, 13.99999999999999645 ) ) ;
#5043 = CARTESIAN_POINT ( 'NONE',  ( 8.256732931686219246, 4.597988481711511533, 1.999999999999998224 ) ) ;
#5044 = DIRECTION ( 'NONE',  ( -1.000000000000000000, -2.664535259100375697E-15, 0.000000000000000000 ) ) ;
#5045 = EDGE_LOOP ( 'NONE', ( #2192, #5116, #1173, #5471 ) ) ;
#5046 = PRODUCT ( 'Spring Coil Unit', 'Spring Coil Unit', '', ( #4397 ) ) ;
#5047 = CARTESIAN_POINT ( 'NONE',  ( 10.50003631213657762, 0.006025845833179020727, 1.999999999999998224 ) ) ;
#5048 = EDGE_LOOP ( 'NONE', ( #3124, #4132, #1685, #1976 ) ) ;
#5049 = FACE_OUTER_BOUND ( 'NONE', #1360, .T. ) ;
#5050 = CARTESIAN_POINT ( 'NONE',  ( -6.876639332705559937, 1.598006320995821516, 14.00000000000000000 ) ) ;
#5051 = CARTESIAN_POINT ( 'NONE',  ( -0.3010823416051303103, -9.281161307073869438, 13.99999999999999645 ) ) ;
#5052 = EDGE_CURVE ( 'NONE', #4608, #1240, #2269, .T. ) ;
#5053 = CARTESIAN_POINT ( 'NONE',  ( -6.881333183081246752, -1.254343363641206688, 14.00000000000000000 ) ) ;
#5054 = ORIENTED_EDGE ( 'NONE', *, *, #1982, .F. ) ;
#5055 = CARTESIAN_POINT ( 'NONE',  ( -3.127066335681005338, 9.214240776399423183, 1.999999999999998224 ) ) ;
#5056 = FACE_OUTER_BOUND ( 'NONE', #4664, .T. ) ;
#5057 = SURFACE_STYLE_FILL_AREA ( #169 ) ;
#5058 = CARTESIAN_POINT ( 'NONE',  ( -6.881333183080980298, -1.254343363641173381, 1.999999999999998224 ) ) ;
#5059 = ORIENTED_EDGE ( 'NONE', *, *, #5186, .T. ) ;
#5060 = CARTESIAN_POINT ( 'NONE',  ( 4.062840028443489793, -5.287223670286648414, 1.999999999999998224 ) ) ;
#5061 = DIRECTION ( 'NONE',  ( 0.000000000000000000, 0.000000000000000000, 1.000000000000000000 ) ) ;
#5062 = CARTESIAN_POINT ( 'NONE',  ( 6.026041665150466464, -0.9817477132364120784, 13.99999999999999645 ) ) ;
#5063 = ADVANCED_FACE ( 'NONE', ( #4028 ), #5212, .F. ) ;
#5064 = CARTESIAN_POINT ( 'NONE',  ( 22.00000000000000000, -2.544261098099317203E-15, 4.000000000000003553 ) ) ;
#5065 = VERTEX_POINT ( 'NONE', #5406 ) ;
#5066 = FACE_OUTER_BOUND ( 'NONE', #192, .T. ) ;
#5067 = LINE ( 'NONE', #703, #1609 ) ;
#5068 = CARTESIAN_POINT ( 'NONE',  ( -2.557952627993305583, -8.967547948950716830, 1.999999999999998224 ) ) ;
#5069 = CARTESIAN_POINT ( 'NONE',  ( -2.263950162103714359, 8.438937471999240714, 13.99999999999999645 ) ) ;
#5070 = DIRECTION ( 'NONE',  ( -1.000000000000000000, 0.000000000000000000, 0.000000000000000000 ) ) ;
#5071 = ORIENTED_EDGE ( 'NONE', *, *, #1454, .F. ) ;
#5072 = DIRECTION ( 'NONE',  ( -1.000000000000000000, 0.000000000000000000, 0.000000000000000000 ) ) ;
#5073 = STYLED_ITEM ( 'NONE', ( #1751 ), #694 ) ;
#5074 = ORIENTED_EDGE ( 'NONE', *, *, #429, .T. ) ;
#5075 = FACE_OUTER_BOUND ( 'NONE', #3066, .T. ) ;
#5076 = CARTESIAN_POINT ( 'NONE',  ( 6.680730669075651385, 3.301097878975988831, 14.00000000000000000 ) ) ;
#5077 = EDGE_CURVE ( 'NONE', #993, #92, #1437, .T. ) ;
#5078 = CARTESIAN_POINT ( 'NONE',  ( 9.599547022228486881, -3.085197981543154278, 13.99999999999999645 ) ) ;
#5079 = EDGE_CURVE ( 'NONE', #4137, #1719, #976, .T. ) ;
#5080 = PRODUCT_DEFINITION_FORMATION_WITH_SPECIFIED_SOURCE ( 'ANY', '', #1195, .NOT_KNOWN. ) ;
#5081 = ADVANCED_FACE ( 'NONE', ( #1026 ), #4599, .F. ) ;
#5082 = CARTESIAN_POINT ( 'NONE',  ( -0.8347742375825083494, 7.207659102801796891, 14.00000000000000000 ) ) ;
#5083 = ORIENTED_EDGE ( 'NONE', *, *, #155, .T. ) ;
#5084 = CARTESIAN_POINT ( 'NONE',  ( -8.483256258862246213, -6.077987531410204980, 1.999999999999998224 ) ) ;
#5085 = DIRECTION ( 'NONE',  ( 0.000000000000000000, 1.000000000000000000, 0.000000000000000000 ) ) ;
#5086 = VECTOR ( 'NONE', #1539, 1000.000000000000000 ) ;
#5087 = CARTESIAN_POINT ( 'NONE',  ( 0.000000000000000000, 0.000000000000000000, 0.000000000000000000 ) ) ;
#5088 = CARTESIAN_POINT ( 'NONE',  ( -5.581220830680290845, 5.949058968288200688, 1.999999999999998224 ) ) ;
#5089 = ORIENTED_EDGE ( 'NONE', *, *, #2928, .F. ) ;
#5090 = EDGE_CURVE ( 'NONE', #2377, #1059, #5347, .T. ) ;
#5091 = CARTESIAN_POINT ( 'NONE',  ( -3.231338468933299790, -7.147216519672494606, 1.999999999999998224 ) ) ;
#5092 = CARTESIAN_POINT ( 'NONE',  ( 0.2194671214740537279, 6.774136816532212890, 1.999999999999998224 ) ) ;
#5093 = CARTESIAN_POINT ( 'NONE',  ( 1.183015137239217696, -7.150809911821260911, 13.99999999999999645 ) ) ;
#5094 = MECHANICAL_DESIGN_GEOMETRIC_PRESENTATION_REPRESENTATION (  '', ( #3171 ), #1601 ) ;
#5095 =( NAMED_UNIT ( * ) SI_UNIT ( $, .STERADIAN. ) SOLID_ANGLE_UNIT ( ) );
#5096 = AXIS2_PLACEMENT_3D ( 'NONE', #5656, #5312, #4788 ) ;
#5097 = DIRECTION ( 'NONE',  ( 1.000000000000000000, 0.000000000000000000, 0.000000000000000000 ) ) ;
#5098 = EDGE_LOOP ( 'NONE', ( #3977, #632, #1923, #1653, #4699 ) ) ;
#5099 = CARTESIAN_POINT ( 'NONE',  ( 1.380000000000002558, 0.000000000000000000, 15.94994774640597512 ) ) ;
#5100 = CARTESIAN_POINT ( 'NONE',  ( 0.1634456542307747284, 10.28566380800474889, 14.00000000000000000 ) ) ;
#5101 = CARTESIAN_POINT ( 'NONE',  ( -5.921118896519414143, 6.318058289644735481, 1.999999999999998224 ) ) ;
#5102 = CIRCLE ( 'NONE', #135, 0.2500000000000002220 ) ;
#5103 = CARTESIAN_POINT ( 'NONE',  ( 8.027649061864064350, -0.2602747315786822502, 13.99999999999999645 ) ) ;
#5104 = EDGE_CURVE ( 'NONE', #5494, #1387, #1049, .T. ) ;
#5105 = DIRECTION ( 'NONE',  ( 0.000000000000000000, 0.000000000000000000, -1.000000000000000000 ) ) ;
#5107 = ORIENTED_EDGE ( 'NONE', *, *, #1274, .F. ) ;
#5106 = COLOUR_RGB ( '',0.8941176470588234615, 0.8941176470588234615, 0.8941176470588234615 ) ;
#5108 = CARTESIAN_POINT ( 'NONE',  ( -5.000000000000000000, 4.999999999999978684, -8.000000000000000000 ) ) ;
#5109 = EDGE_CURVE ( 'NONE', #4504, #1983, #5286, .T. ) ;
#5110 = VERTEX_POINT ( 'NONE', #5028 ) ;
#5111 = LINE ( 'NONE', #1133, #159 ) ;
#5112 = CARTESIAN_POINT ( 'NONE',  ( 5.053476174606819527, -5.757900651972699180, 14.00000000000000000 ) ) ;
#5113 = ADVANCED_FACE ( 'NONE', ( #3221 ), #3595, .T. ) ;
#5114 = CARTESIAN_POINT ( 'NONE',  ( -9.247243397275783039, 2.478494142799223976, 13.99999999999999645 ) ) ;
#5115 = CARTESIAN_POINT ( 'NONE',  ( 5.733165789232424814, 2.946509839760390381, 14.00000000000000000 ) ) ;
#5116 = ORIENTED_EDGE ( 'NONE', *, *, #4947, .T. ) ;
#5117 = CIRCLE ( 'NONE', #706, 2.149999999999998579 ) ;
#5118 = CARTESIAN_POINT ( 'NONE',  ( -9.026614039607443019, -2.903226997913650465, 1.999999999999998224 ) ) ;
#5119 = CARTESIAN_POINT ( 'NONE',  ( 3.885274725274726393, -8.673617379884035472E-16, 0.000000000000000000 ) ) ;
#5120 = AXIS2_PLACEMENT_3D ( 'NONE', #2503, #5558, #3346 ) ;
#5121 =( NAMED_UNIT ( * ) PLANE_ANGLE_UNIT ( ) SI_UNIT ( $, .RADIAN. ) );
#5122 = CARTESIAN_POINT ( 'NONE',  ( 2.543939756934456842, 7.929199913827334356, 1.999999999999998224 ) ) ;
#5123 = DIRECTION ( 'NONE',  ( -1.000000000000000000, 0.000000000000000000, 0.000000000000000000 ) ) ;
#5124 = VECTOR ( 'NONE', #2877, 999.9999999999998863 ) ;
#5125 = CARTESIAN_POINT ( 'NONE',  ( 3.909482108038855319, 5.648312977191786821, 13.99999999999999645 ) ) ;
#5126 = EDGE_CURVE ( 'NONE', #2224, #442, #4968, .T. ) ;
#5127 = AXIS2_PLACEMENT_3D ( 'NONE', #1782, #3482, #2624 ) ;
#5128 = CARTESIAN_POINT ( 'NONE',  ( 0.000000000000000000, 0.000000000000000000, 8.000000000000000000 ) ) ;
#5129 = PLANE ( 'NONE',  #4187 ) ;
#5130 = VERTEX_POINT ( 'NONE', #4916 ) ;
#5131 = DIRECTION ( 'NONE',  ( -0.000000000000000000, -0.000000000000000000, -1.000000000000000000 ) ) ;
#5132 = DIRECTION ( 'NONE',  ( -1.000000000000000000, 0.000000000000000000, 0.000000000000000000 ) ) ;
#5133 = CARTESIAN_POINT ( 'NONE',  ( -9.247243397276459831, 2.478494142799053446, 1.999999999999998224 ) ) ;
#5134 = CARTESIAN_POINT ( 'NONE',  ( 9.020117466465418232, 0.2947087185667972564, 13.99999999999999645 ) ) ;
#5135 = CARTESIAN_POINT ( 'NONE',  ( 0.000000000000000000, 0.000000000000000000, 12.00000000000000000 ) ) ;
#5136 = EDGE_LOOP ( 'NONE', ( #766, #117, #1602, #3548 ) ) ;
#5137 = CARTESIAN_POINT ( 'NONE',  ( -22.50000000000000355, 0.000000000000000000, 14.00000000000000000 ) ) ;
#5138 = ORIENTED_EDGE ( 'NONE', *, *, #4766, .T. ) ;
#5139 = FACE_BOUND ( 'NONE', #3150, .T. ) ;
#5140 = CARTESIAN_POINT ( 'NONE',  ( -6.317162512442926037, 3.238855812894408714, 14.00000000000000000 ) ) ;
#5141 = CARTESIAN_POINT ( 'NONE',  ( -9.742306995815035009, -3.848972158781221786, 13.99999999999999645 ) ) ;
#5142 = CARTESIAN_POINT ( 'NONE',  ( -3.597458971453999954, 6.226096630968013912, 14.00000000000000000 ) ) ;
#5143 = ORIENTED_EDGE ( 'NONE', *, *, #4, .F. ) ;
#5144 = CARTESIAN_POINT ( 'NONE',  ( -2.557952627993305583, -8.967547948950716830, 1.999999999999998224 ) ) ;
#5145 = PRODUCT ( 'outer cover 1', 'outer cover 1', '', ( #2693 ) ) ;
#5146 = EDGE_CURVE ( 'NONE', #1251, #5065, #43, .T. ) ;
#5147 = CARTESIAN_POINT ( 'NONE',  ( 0.000000000000000000, 0.000000000000000000, 3.799999999999999378 ) ) ;
#5148 = DIRECTION ( 'NONE',  ( 0.000000000000000000, 0.000000000000000000, 1.000000000000000000 ) ) ;
#5149 = CARTESIAN_POINT ( 'NONE',  ( -3.231338468933299790, -7.147216519672494606, 1.999999999999998224 ) ) ;
#5150 = DIRECTION ( 'NONE',  ( -1.000000000000000000, -0.000000000000000000, -0.000000000000000000 ) ) ;
#5151 = CARTESIAN_POINT ( 'NONE',  ( 1.015216742983949372, 7.730330528320555672, 13.99999999999999645 ) ) ;
#5152 = SURFACE_STYLE_FILL_AREA ( #4259 ) ;
#5153 = CARTESIAN_POINT ( 'NONE',  ( 8.172274133037948474, -5.076547540501181288, 1.999999999999998224 ) ) ;
#5154 = CARTESIAN_POINT ( 'NONE',  ( -5.000000000000085265, 24.49489742783176638, -8.000000000000000000 ) ) ;
#5155 = VERTEX_POINT ( 'NONE', #2734 ) ;
#5156 = DIRECTION ( 'NONE',  ( -1.000000000000000000, 0.000000000000000000, -0.000000000000000000 ) ) ;
#5157 = DIRECTION ( 'NONE',  ( 0.000000000000000000, 2.258754526011467828E-18, -1.000000000000000000 ) ) ;
#5158 = CARTESIAN_POINT ( 'NONE',  ( -9.406456921418632433, 1.708717176649267477, 13.99999999999999645 ) ) ;
#5159 = CARTESIAN_POINT ( 'NONE',  ( -0.6809175113353355124, 10.25113960786383949, 14.00000000000000000 ) ) ;
#5160 = ORIENTED_EDGE ( 'NONE', *, *, #2367, .T. ) ;
#5161 = DIRECTION ( 'NONE',  ( 0.000000000000000000, 0.000000000000000000, 1.000000000000000000 ) ) ;
#5162 = ORIENTED_EDGE ( 'NONE', *, *, #1380, .T. ) ;
#5163 = DIRECTION ( 'NONE',  ( -1.000000000000000000, 0.000000000000000000, 0.000000000000000000 ) ) ;
#5164 = CARTESIAN_POINT ( 'NONE',  ( 7.320916985966520407, 1.587212364775818285, 14.00000000000000000 ) ) ;
#5165 = CARTESIAN_POINT ( 'NONE',  ( -3.287100391418014578, 10.22059872437975869, 13.99999999999999645 ) ) ;
#5166 = CARTESIAN_POINT ( 'NONE',  ( 6.445330636073146380, -1.168293168414177741, 14.00000000000000000 ) ) ;
#5167 = ORIENTED_EDGE ( 'NONE', *, *, #3555, .F. ) ;
#5168 = CARTESIAN_POINT ( 'NONE',  ( 7.775655769254118610, 6.170250810330676572, 1.999999999999998224 ) ) ;
#5169 = EDGE_CURVE ( 'NONE', #1307, #1462, #1237, .T. ) ;
#5170 = DIRECTION ( 'NONE',  ( -1.000000000000000000, 0.000000000000000000, -0.000000000000000000 ) ) ;
#5171 = CARTESIAN_POINT ( 'NONE',  ( 7.280083392764698402, -2.072676875633882254, 1.999999999999998224 ) ) ;
#5172 = DIRECTION ( 'NONE',  ( 0.000000000000000000, 0.000000000000000000, -1.000000000000000000 ) ) ;
#5173 = CARTESIAN_POINT ( 'NONE',  ( 2.877506500681688895, 7.288437455188075731, 13.99999999999999645 ) ) ;
#5174 = ADVANCED_FACE ( 'NONE', ( #2293 ), #136, .T. ) ;
#5175 = CARTESIAN_POINT ( 'NONE',  ( 3.433597602020624251, -9.098706718023301221, 1.999999999999998224 ) ) ;
#5176 = EDGE_CURVE ( 'NONE', #2002, #3324, #5380, .T. ) ;
#5177 = CARTESIAN_POINT ( 'NONE',  ( 5.500000000000001776, 0.000000000000000000, 14.00000000000000000 ) ) ;
#5178 = MECHANICAL_DESIGN_GEOMETRIC_PRESENTATION_REPRESENTATION (  '', ( #3986 ), #2516 ) ;
#5179 = DIRECTION ( 'NONE',  ( 1.000000000000000000, 0.000000000000000000, 0.000000000000000000 ) ) ;
#5180 = VERTEX_POINT ( 'NONE', #2380 ) ;
#5181 = DIRECTION ( 'NONE',  ( -1.000000000000000000, 0.000000000000000000, 0.000000000000000000 ) ) ;
#5182 = DIRECTION ( 'NONE',  ( -1.000000000000000000, 0.000000000000000000, 0.000000000000000000 ) ) ;
#5183 = EDGE_CURVE ( 'NONE', #3426, #3736, #2761, .T. ) ;
#5184 = AXIS2_PLACEMENT_3D ( 'NONE', #3684, #1494, #4036 ) ;
#5185 = CARTESIAN_POINT ( 'NONE',  ( -9.247243397275783039, 2.478494142799223976, 13.99999999999999645 ) ) ;
#5186 = EDGE_CURVE ( 'NONE', #5180, #928, #4514, .T. ) ;
#5187 = CARTESIAN_POINT ( 'NONE',  ( 8.673617379884035472E-16, 1.899999999999999689, 0.000000000000000000 ) ) ;
#5188 = ORIENTED_EDGE ( 'NONE', *, *, #925, .T. ) ;
#5189 = LINE ( 'NONE', #2570, #2343 ) ;
#5190 = ORIENTED_EDGE ( 'NONE', *, *, #1872, .F. ) ;
#5191 = CARTESIAN_POINT ( 'NONE',  ( 1.300000000000000044, 0.7216878364870328300, -1.250000000000000000 ) ) ;
#5192 = VECTOR ( 'NONE', #3276, 1000.000000000000000 ) ;
#5193 = CARTESIAN_POINT ( 'NONE',  ( 1.853537052132013807, -8.546502713975392851, 14.00000000000000000 ) ) ;
#5194 = CARTESIAN_POINT ( 'NONE',  ( 9.199536834907137361, 5.930433524308741156, 13.99999999999999645 ) ) ;
#5195 = ADVANCED_FACE ( 'NONE', ( #565 ), #4082, .F. ) ;
#5196 = CIRCLE ( 'NONE', #1243, 2.149999999999998579 ) ;
#5197 = DIRECTION ( 'NONE',  ( 0.000000000000000000, 0.000000000000000000, 1.000000000000000000 ) ) ;
#5198 = CARTESIAN_POINT ( 'NONE',  ( -0.1423371034015828429, 8.273642750286580139, 14.00000000000000000 ) ) ;
#5199 = ORIENTED_EDGE ( 'NONE', *, *, #5614, .F. ) ;
#5200 = CARTESIAN_POINT ( 'NONE',  ( -9.197478219253614640, 5.306711421960435437, 1.999999999999998224 ) ) ;
#5201 = AXIS2_PLACEMENT_3D ( 'NONE', #709, #213, #5072 ) ;
#5202 = CARTESIAN_POINT ( 'NONE',  ( -5.402835942920536816, -5.063607225391134392, 13.99999999999999645 ) ) ;
#5203 = FILL_AREA_STYLE ('',( #1206 ) ) ;
#5204 = CARTESIAN_POINT ( 'NONE',  ( -3.813875884798381577, -6.869235835554530212, 1.999999999999998224 ) ) ;
#5205 = VECTOR ( 'NONE', #1385, 1000.000000000000000 ) ;
#5206 = DIRECTION ( 'NONE',  ( -0.000000000000000000, -0.000000000000000000, 1.000000000000000000 ) ) ;
#5207 = AXIS2_PLACEMENT_3D ( 'NONE', #1823, #5279, #1335 ) ;
#5208 = CARTESIAN_POINT ( 'NONE',  ( 6.938542625487071902, -1.260128425111980643, 13.99999999999999645 ) ) ;
#5209 = PRODUCT_DEFINITION ( 'UNKNOWN', '', #3610, #4761 ) ;
#5210 = CLOSED_SHELL ( 'NONE', ( #5356, #3334, #312, #3138, #5627, #4832, #1954, #1943, #2265, #775, #5364, #2793 ) ) ;
#5211 = AXIS2_PLACEMENT_3D ( 'NONE', #1587, #727, #5156 ) ;
#5212 = CYLINDRICAL_SURFACE ( 'NONE', #1604, 2.149999999999998579 ) ;
#5213 = DIRECTION ( 'NONE',  ( 1.000000000000000000, 0.000000000000000000, 0.000000000000000000 ) ) ;
#5214 = CARTESIAN_POINT ( 'NONE',  ( -7.161907081466631908, 5.673982509928833018, 1.999999999999998224 ) ) ;
#5215 =( GEOMETRIC_REPRESENTATION_CONTEXT ( 3 ) GLOBAL_UNCERTAINTY_ASSIGNED_CONTEXT ( ( #5354 ) ) GLOBAL_UNIT_ASSIGNED_CONTEXT ( ( #2356, #5498, #605 ) ) REPRESENTATION_CONTEXT ( 'NONE', 'WORKASPACE' ) );
#5216 = CARTESIAN_POINT ( 'NONE',  ( 0.000000000000000000, 0.000000000000000000, 8.000000000000000000 ) ) ;
#5217 = LINE ( 'NONE', #2478, #968 ) ;
#5218 = VERTEX_POINT ( 'NONE', #4139 ) ;
#5219 = DIRECTION ( 'NONE',  ( -0.000000000000000000, -0.000000000000000000, -1.000000000000000000 ) ) ;
#5220 = CARTESIAN_POINT ( 'NONE',  ( 1.380000000000002558, 0.000000000000000000, 12.00000000000000000 ) ) ;
#5221 = CIRCLE ( 'NONE', #1637, 2.199999999999999289 ) ;
#5222 = CARTESIAN_POINT ( 'NONE',  ( 7.233280636258937690, 6.778630567624380099, 13.99999999999999645 ) ) ;
#5223 = DIRECTION ( 'NONE',  ( 0.000000000000000000, 0.000000000000000000, -1.000000000000000000 ) ) ;
#5224 = ORIENTED_EDGE ( 'NONE', *, *, #1094, .T. ) ;
#5225 = LINE ( 'NONE', #4754, #877 ) ;
#5226 = ORIENTED_EDGE ( 'NONE', *, *, #2017, .T. ) ;
#5227 = LINE ( 'NONE', #1739, #1723 ) ;
#5228 = CARTESIAN_POINT ( 'NONE',  ( -5.081985621531964981, 6.397721742171718518, 14.00000000000000000 ) ) ;
#5229 = CARTESIAN_POINT ( 'NONE',  ( 3.909482108038854431, 5.648312977191785045, 1.999999999999998224 ) ) ;
#5230 = UNCERTAINTY_MEASURE_WITH_UNIT (LENGTH_MEASURE( 1.000000000000000082E-05 ), #2989, 'distance_accuracy_value', 'NONE');
#5231 = DIRECTION ( 'NONE',  ( -1.000000000000000000, -0.000000000000000000, -0.000000000000000000 ) ) ;
#5232 = CARTESIAN_POINT ( 'NONE',  ( 0.5385325299235224072, 8.270587056550175120, 14.00000000000000000 ) ) ;
#5233 = ORIENTED_EDGE ( 'NONE', *, *, #4902, .T. ) ;
#5234 = DIRECTION ( 'NONE',  ( 0.000000000000000000, 0.000000000000000000, 1.000000000000000000 ) ) ;
#5235 = EDGE_CURVE ( 'NONE', #1305, #2861, #629, .T. ) ;
#5236 = CARTESIAN_POINT ( 'NONE',  ( 4.366464973618273682, -5.686602709308030690, 13.99999999999999645 ) ) ;
#5237 = CONTEXT_DEPENDENT_SHAPE_REPRESENTATION ( #5632, #2619 ) ;
#5238 = CARTESIAN_POINT ( 'NONE',  ( -5.592500163775054212, 7.275211197852026856, 1.999999999999998224 ) ) ;
#5239 = CARTESIAN_POINT ( 'NONE',  ( 4.366464973618271905, -5.686602709308029802, 1.999999999999998224 ) ) ;
#5240 = CARTESIAN_POINT ( 'NONE',  ( -8.513020831365363250, 0.6954046021538080602, 13.99999999999999645 ) ) ;
#5241 = DIRECTION ( 'NONE',  ( 0.000000000000000000, 0.000000000000000000, 1.000000000000000000 ) ) ;
#5242 = SURFACE_STYLE_FILL_AREA ( #26 ) ;
#5243 = CARTESIAN_POINT ( 'NONE',  ( 1.300000000000000044, -1.443375672974063884, -3.691112476943992763E-18 ) ) ;
#5244 = PLANE ( 'NONE',  #2077 ) ;
#5245 = CARTESIAN_POINT ( 'NONE',  ( 21.75000000000000000, -3.307189138830739061, 4.000000000000001776 ) ) ;
#5246 = EDGE_LOOP ( 'NONE', ( #1579, #4548, #2479, #2502 ) ) ;
#5247 =( LENGTH_UNIT ( ) NAMED_UNIT ( * ) SI_UNIT ( .MILLI., .METRE. ) );
#5248 = CARTESIAN_POINT ( 'NONE',  ( 8.993528569561179964, -4.616306094804236260, 13.99999999999999645 ) ) ;
#5249 =( LENGTH_UNIT ( ) NAMED_UNIT ( * ) SI_UNIT ( .MILLI., .METRE. ) );
#5250 = ORIENTED_EDGE ( 'NONE', *, *, #2535, .T. ) ;
#5251 = CARTESIAN_POINT ( 'NONE',  ( 1.300000000000000044, -1.443375672974063884, -3.691112476943992763E-18 ) ) ;
#5252 = ORIENTED_EDGE ( 'NONE', *, *, #4420, .F. ) ;
#5253 = LINE ( 'NONE', #1308, #3196 ) ;
#5254 = CARTESIAN_POINT ( 'NONE',  ( -6.667513054348625623, -4.302816426345352774, 14.00000000000000000 ) ) ;
#5255 = CARTESIAN_POINT ( 'NONE',  ( -6.045729098460493667, -8.441868823237593134, 13.99999999999999645 ) ) ;
#5256 = CARTESIAN_POINT ( 'NONE',  ( 0.000000000000000000, 0.000000000000000000, 2.000000000000000000 ) ) ;
#5257 = CARTESIAN_POINT ( 'NONE',  ( 3.857245400775171529, -7.804869966781184054, 14.00000000000000000 ) ) ;
#5258 = EDGE_CURVE ( 'NONE', #4992, #2140, #2709, .T. ) ;
#5259 = ORIENTED_EDGE ( 'NONE', *, *, #975, .T. ) ;
#5260 = DIRECTION ( 'NONE',  ( 1.000000000000000000, 0.000000000000000000, -0.000000000000000000 ) ) ;
#5261 = SHAPE_REPRESENTATION ( 'Spool Drum', ( #1336 ), #3360 ) ;
#5262 = CARTESIAN_POINT ( 'NONE',  ( -5.978927507574435474, 2.933119789328458182, 13.99999999999999645 ) ) ;
#5263 = CARTESIAN_POINT ( 'NONE',  ( -8.757712506721389900, -2.046213373001789737, 1.999999999999998224 ) ) ;
#5264 = CARTESIAN_POINT ( 'NONE',  ( -3.845892476879857025, 6.661954734853423155, 1.999999999999998224 ) ) ;
#5265 = CARTESIAN_POINT ( 'NONE',  ( 0.000000000000000000, 0.000000000000000000, 5.000000000000000000 ) ) ;
#5266 = ADVANCED_FACE ( 'NONE', ( #1009, #637 ), #3228, .F. ) ;
#5267 = CARTESIAN_POINT ( 'NONE',  ( 21.74999999999999645, -30.00000000000000000, 12.00000000000000000 ) ) ;
#5268 = EDGE_CURVE ( 'NONE', #2258, #4732, #3335, .T. ) ;
#5269 = CARTESIAN_POINT ( 'NONE',  ( 5.500000000000000000, 0.000000000000000000, 1.999999999999998224 ) ) ;
#5270 = CARTESIAN_POINT ( 'NONE',  ( 0.000000000000000000, 0.000000000000000000, 14.00000000000000000 ) ) ;
#5271 = ORIENTED_EDGE ( 'NONE', *, *, #2632, .F. ) ;
#5272 = CARTESIAN_POINT ( 'NONE',  ( 5.000000000000000000, 5.000000000000022204, -8.000000000000000000 ) ) ;
#5273 = DIRECTION ( 'NONE',  ( -0.000000000000000000, -0.000000000000000000, -1.000000000000000000 ) ) ;
#5274 = VECTOR ( 'NONE', #2568, 1000.000000000000000 ) ;
#5275 = SURFACE_STYLE_USAGE ( .BOTH. , #2166 ) ;
#5276 = ORIENTED_EDGE ( 'NONE', *, *, #4924, .T. ) ;
#5277 = FACE_OUTER_BOUND ( 'NONE', #3679, .T. ) ;
#5278 = EDGE_LOOP ( 'NONE', ( #3810, #5054 ) ) ;
#5279 = DIRECTION ( 'NONE',  ( -0.000000000000000000, -0.000000000000000000, 1.000000000000000000 ) ) ;
#5280 = CARTESIAN_POINT ( 'NONE',  ( 6.037635170864974477, 5.848285684831325604, 14.00000000000000000 ) ) ;
#5281 = CARTESIAN_POINT ( 'NONE',  ( -7.364573508975982286, 1.714675912027187943, 1.999999999999998224 ) ) ;
#5282 = COLOUR_RGB ( '',0.8941176470588234615, 0.8941176470588234615, 0.8941176470588234615 ) ;
#5283 = EDGE_CURVE ( 'NONE', #4410, #4643, #223, .T. ) ;
#5284 = CARTESIAN_POINT ( 'NONE',  ( -15.00000000000000000, 0.000000000000000000, 12.00000000000000000 ) ) ;
#5285 = CARTESIAN_POINT ( 'NONE',  ( 5.612687125618119666, -6.603876269260188892, 14.00000000000000000 ) ) ;
#5286 = CIRCLE ( 'NONE', #3715, 1.610000000000000098 ) ;
#5287 = ORIENTED_EDGE ( 'NONE', *, *, #3416, .T. ) ;
#5288 = CARTESIAN_POINT ( 'NONE',  ( -7.551678268146208239, 5.989845445213456188, 1.999999999999998224 ) ) ;
#5289 = CARTESIAN_POINT ( 'NONE',  ( 0.000000000000000000, 0.000000000000000000, -8.000000000000000000 ) ) ;
#5290 = CARTESIAN_POINT ( 'NONE',  ( -2.352725117874390648, -6.938351456669185069, 13.99999999999999645 ) ) ;
#5291 = SHAPE_DEFINITION_REPRESENTATION ( #409, #5261 ) ;
#5292 = CARTESIAN_POINT ( 'NONE',  ( 5.071900148311750733, 7.881338450276374807, 1.999999999999998224 ) ) ;
#5293 = CARTESIAN_POINT ( 'NONE',  ( 6.180183843827202317, 3.174252413088801461, 1.999999999999998224 ) ) ;
#5294 = CYLINDRICAL_SURFACE ( 'NONE', #496, 25.00000000000000355 ) ;
#5295 = AXIS2_PLACEMENT_3D ( 'NONE', #5216, #400, #4321 ) ;
#5296 = CARTESIAN_POINT ( 'NONE',  ( 5.526041665711819206, -0.8982374663919266977, 1.999999999999998224 ) ) ;
#5297 = DIRECTION ( 'NONE',  ( -0.000000000000000000, -0.000000000000000000, -1.000000000000000000 ) ) ;
#5298 = CARTESIAN_POINT ( 'NONE',  ( 23.00000000000000000, -8.144275775193202933E-15, -4.000000000000000000 ) ) ;
#5299 = ORIENTED_EDGE ( 'NONE', *, *, #5501, .T. ) ;
#5300 = AXIS2_PLACEMENT_3D ( 'NONE', #2419, #2799, #1013 ) ;
#5301 = CARTESIAN_POINT ( 'NONE',  ( 0.000000000000000000, 0.000000000000000000, 4.000000000000000000 ) ) ;
#5302 = ADVANCED_FACE ( 'NONE', ( #5547 ), #5604, .T. ) ;
#5303 = CARTESIAN_POINT ( 'NONE',  ( 10.02239396097876423, -0.6576683464575836524, 13.99999999999999645 ) ) ;
#5304 = AXIS2_PLACEMENT_3D ( 'NONE', #3300, #2004, #1595 ) ;
#5305 = LINE ( 'NONE', #5616, #4805 ) ;
#5306 = DIRECTION ( 'NONE',  ( 0.000000000000000000, 0.000000000000000000, 1.000000000000000000 ) ) ;
#5307 = ORIENTED_EDGE ( 'NONE', *, *, #3561, .F. ) ;
#5308 = VERTEX_POINT ( 'NONE', #1552 ) ;
#5309 = CARTESIAN_POINT ( 'NONE',  ( -5.048038583874033591, -7.300734008993382318, 14.00000000000000000 ) ) ;
#5310 = CARTESIAN_POINT ( 'NONE',  ( 6.209839678910233474, -3.451293940533043614, 1.999999999999998224 ) ) ;
#5311 = VECTOR ( 'NONE', #3879, 1000.000000000000000 ) ;
#5312 = DIRECTION ( 'NONE',  ( -0.000000000000000000, -0.000000000000000000, 1.000000000000000000 ) ) ;
#5313 = CARTESIAN_POINT ( 'NONE',  ( -1.390902631672706224, -7.679604985168660747, 14.00000000000000000 ) ) ;
#5314 = AXIS2_PLACEMENT_3D ( 'NONE', #421, #2180, #4819 ) ;
#5315 = EDGE_LOOP ( 'NONE', ( #3867, #5287, #1468, #4118, #2138, #3008 ) ) ;
#5316 = CARTESIAN_POINT ( 'NONE',  ( -10.26372689808571970, -2.219791875069699216, 1.999999999999998224 ) ) ;
#5317 = CARTESIAN_POINT ( 'NONE',  ( 8.671201137383034663, 6.657490096169006222, 1.999999999999998224 ) ) ;
#5318 = CARTESIAN_POINT ( 'NONE',  ( -2.919577271296576182, -6.733962781534541975, 13.99999999999999645 ) ) ;
#5319 = SHAPE_DEFINITION_REPRESENTATION ( #2426, #3487 ) ;
#5320 = CARTESIAN_POINT ( 'NONE',  ( 1.124407659250306279, -9.699258357302506184, 1.999999999999998224 ) ) ;
#5321 = CARTESIAN_POINT ( 'NONE',  ( -2.352725117874390204, -6.938351456669183293, 1.999999999999998224 ) ) ;
#5322 = SURFACE_SIDE_STYLE ('',( #3566 ) ) ;
#5323 = DIRECTION ( 'NONE',  ( -0.000000000000000000, -0.000000000000000000, 1.000000000000000000 ) ) ;
#5324 = CARTESIAN_POINT ( 'NONE',  ( 10.36702220812592223, 1.720931399333113676, 1.999999999999998224 ) ) ;
#5325 = CARTESIAN_POINT ( 'NONE',  ( -5.000000000000000000, 0.000000000000000000, 8.000000000000000000 ) ) ;
#5326 = CARTESIAN_POINT ( 'NONE',  ( 1.300000000000000044, 1.082531754730548856, 0.6250000000000006661 ) ) ;
#5327 = ORIENTED_EDGE ( 'NONE', *, *, #5662, .T. ) ;
#5328 = ADVANCED_FACE ( 'NONE', ( #1143 ), #3792, .T. ) ;
#5329 = DIRECTION ( 'NONE',  ( 2.385244779468107388E-15, 1.000000000000000000, 0.000000000000000000 ) ) ;
#5330 = DIRECTION ( 'NONE',  ( 1.000000000000000000, 0.000000000000000000, 0.000000000000000000 ) ) ;
#5331 =( LENGTH_UNIT ( ) NAMED_UNIT ( * ) SI_UNIT ( .MILLI., .METRE. ) );
#5332 = LINE ( 'NONE', #4841, #3368 ) ;
#5333 = ORIENTED_EDGE ( 'NONE', *, *, #4407, .T. ) ;
#5334 = ORIENTED_EDGE ( 'NONE', *, *, #4247, .F. ) ;
#5335 = CARTESIAN_POINT ( 'NONE',  ( -2.970508497641844325, 8.737606122599315128, 14.00000000000000000 ) ) ;
#5336 = CARTESIAN_POINT ( 'NONE',  ( -6.505530684480364201, -3.618119970335912150, 1.999999999999998224 ) ) ;
#5337 = CARTESIAN_POINT ( 'NONE',  ( 8.370269057507494281, -1.803949267857694716, 1.999999999999998224 ) ) ;
#5338 = CARTESIAN_POINT ( 'NONE',  ( 5.519166806814065573, -7.959527472086049826, 14.00000000000000000 ) ) ;
#5339 = VERTEX_POINT ( 'NONE', #3732 ) ;
#5340 = CARTESIAN_POINT ( 'NONE',  ( -10.17357856257854110, 2.902115915870757679, 1.999999999999998224 ) ) ;
#5341 = CARTESIAN_POINT ( 'NONE',  ( -0.3669926094919908621, -5.824518274481599533, 14.00000000000000000 ) ) ;
#5342 = CARTESIAN_POINT ( 'NONE',  ( 6.033242055734853615, 5.122103984031451063, 13.99999999999999645 ) ) ;
#5343 = CARTESIAN_POINT ( 'NONE',  ( -0.8890388043606451962, 7.706404363472290520, 13.99999999999999645 ) ) ;
#5344 = CARTESIAN_POINT ( 'NONE',  ( -7.161907081466631908, 5.673982509928833018, 1.999999999999998224 ) ) ;
#5345 = ORIENTED_EDGE ( 'NONE', *, *, #4090, .T. ) ;
#5346 = CARTESIAN_POINT ( 'NONE',  ( 8.640499015841685448, 2.466831329604985079, 1.999999999999998224 ) ) ;
#5347 = LINE ( 'NONE', #1517, #5192 ) ;
#5348 = PRODUCT_RELATED_PRODUCT_CATEGORY ( 'part', '', ( #5145 ) ) ;
#5349 =( NAMED_UNIT ( * ) PLANE_ANGLE_UNIT ( ) SI_UNIT ( $, .RADIAN. ) );
#5350 = CARTESIAN_POINT ( 'NONE',  ( 3.885274725274726393, -8.673617379884035472E-16, 0.000000000000000000 ) ) ;
#5351 = CARTESIAN_POINT ( 'NONE',  ( -0.8169484412210608060, 6.196426872864403634, 1.999999999999998224 ) ) ;
#5352 = DIRECTION ( 'NONE',  ( -1.000000000000000000, -0.000000000000000000, -0.000000000000000000 ) ) ;
#5353 = SURFACE_STYLE_FILL_AREA ( #3600 ) ;
#5354 = UNCERTAINTY_MEASURE_WITH_UNIT (LENGTH_MEASURE( 1.000000000000000082E-05 ), #2356, 'distance_accuracy_value', 'NONE');
#5355 = CARTESIAN_POINT ( 'NONE',  ( -4.892757975385814362, 9.527326283048992650, 13.99999999999999645 ) ) ;
#5356 = ADVANCED_FACE ( 'NONE', ( #5056 ), #2901, .T. ) ;
#5357 = CARTESIAN_POINT ( 'NONE',  ( -5.000000000000076383, 22.44994432064363110, 8.000000000000000000 ) ) ;
#5358 = DIRECTION ( 'NONE',  ( 0.000000000000000000, 0.000000000000000000, 1.000000000000000000 ) ) ;
#5359 = AXIS2_PLACEMENT_3D ( 'NONE', #4661, #3507, #21 ) ;
#5360 = ORIENTED_EDGE ( 'NONE', *, *, #4686, .F. ) ;
#5361 = VERTEX_POINT ( 'NONE', #686 ) ;
#5362 = CARTESIAN_POINT ( 'NONE',  ( 1.511842404626676961, 9.183516746439467582, 14.00000000000000000 ) ) ;
#5363 = CARTESIAN_POINT ( 'NONE',  ( 6.679452517770526399, -4.623421500472435497, 1.999999999999998224 ) ) ;
#5364 = ADVANCED_FACE ( 'NONE', ( #2438, #4200 ), #4654, .F. ) ;
#5365 = CARTESIAN_POINT ( 'NONE',  ( 1.147089839255700294, -8.682979827541576157, 1.999999999999998224 ) ) ;
#5366 = CARTESIAN_POINT ( 'NONE',  ( 2.678407690932720353, -9.362678857628843332, 14.00000000000000000 ) ) ;
#5367 = ORIENTED_EDGE ( 'NONE', *, *, #412, .F. ) ;
#5368 = CARTESIAN_POINT ( 'NONE',  ( 5.348203032363056053, 8.300083771889280371, 1.999999999999998224 ) ) ;
#5369 = AXIS2_PLACEMENT_3D ( 'NONE', #4269, #5479, #212 ) ;
#5370 = PLANE ( 'NONE',  #2553 ) ;
#5371 = CARTESIAN_POINT ( 'NONE',  ( 8.640499015841685448, 2.466831329604985079, 13.99999999999999645 ) ) ;
#5372 = EDGE_CURVE ( 'NONE', #3309, #5218, #4915, .T. ) ;
#5373 = CARTESIAN_POINT ( 'NONE',  ( -8.440272934376814362, 1.393994921405934173, 13.99999999999999645 ) ) ;
#5374 = CIRCLE ( 'NONE', #2704, 25.00000000000000000 ) ;
#5375 = CARTESIAN_POINT ( 'NONE',  ( -5.525185448606695360, 2.707100724334913444, 14.00000000000000000 ) ) ;
#5376 = VERTEX_POINT ( 'NONE', #252 ) ;
#5377 = CARTESIAN_POINT ( 'NONE',  ( 8.859712399100347469, -1.914114158827000312, 1.999999999999998224 ) ) ;
#5378 = FACE_OUTER_BOUND ( 'NONE', #3935, .T. ) ;
#5379 = AXIS2_PLACEMENT_3D ( 'NONE', #4996, #5432, #1487 ) ;
#5380 = LINE ( 'NONE', #4945, #2895 ) ;
#5381 = CARTESIAN_POINT ( 'NONE',  ( 0.7175617537426045578, 6.248173425771537559, 1.999999999999998224 ) ) ;
#5382 = CIRCLE ( 'NONE', #2992, 0.2500000000000002220 ) ;
#5383 = ORIENTED_EDGE ( 'NONE', *, *, #4059, .T. ) ;
#5384 = FACE_OUTER_BOUND ( 'NONE', #1440, .T. ) ;
#5385 = DIRECTION ( 'NONE',  ( 0.000000000000000000, 0.000000000000000000, 1.000000000000000000 ) ) ;
#5386 = CARTESIAN_POINT ( 'NONE',  ( -5.623512120026317618, -3.262381593763366450, 13.99999999999999645 ) ) ;
#5387 = VECTOR ( 'NONE', #285, 1000.000000000000000 ) ;
#5388 =( LENGTH_UNIT ( ) NAMED_UNIT ( * ) SI_UNIT ( .MILLI., .METRE. ) );
#5389 = VECTOR ( 'NONE', #955, 1000.000000000000000 ) ;
#5390 = CARTESIAN_POINT ( 'NONE',  ( 22.50000000000000355, 2.755455298081545172E-15, 14.00000000000000000 ) ) ;
#5391 = ORIENTED_EDGE ( 'NONE', *, *, #2700, .F. ) ;
#5392 = VERTEX_POINT ( 'NONE', #2929 ) ;
#5393 = CARTESIAN_POINT ( 'NONE',  ( -4.983290658054754019, 7.721050520723660604, 14.00000000000000000 ) ) ;
#5394 = CARTESIAN_POINT ( 'NONE',  ( 6.938542625487070126, -1.260128425111949557, 1.999999999999998224 ) ) ;
#5395 = CARTESIAN_POINT ( 'NONE',  ( 2.543939756934456842, 7.929199913827334356, 1.999999999999998224 ) ) ;
#5396 = CARTESIAN_POINT ( 'NONE',  ( -9.273719170356997665, -3.669762015051720727, 14.00000000000000000 ) ) ;
#5397 = VERTEX_POINT ( 'NONE', #2011 ) ;
#5398 = AXIS2_PLACEMENT_3D ( 'NONE', #1386, #3969, #402 ) ;
#5399 = CARTESIAN_POINT ( 'NONE',  ( 8.993528569561179964, -4.616306094804414784, 1.999999999999998224 ) ) ;
#5400 = CARTESIAN_POINT ( 'NONE',  ( -5.637968025906140213, -2.116521738900702942, 14.00000000000000000 ) ) ;
#5401 = CARTESIAN_POINT ( 'NONE',  ( 4.043470907200354070, 7.877814422642792636, 13.99999999999999645 ) ) ;
#5402 = CIRCLE ( 'NONE', #619, 4.324969328314201888 ) ;
#5403 = CARTESIAN_POINT ( 'NONE',  ( 1.730265954310492571, 6.073542049876724747, 14.00000000000000000 ) ) ;
#5404 = ORIENTED_EDGE ( 'NONE', *, *, #5546, .T. ) ;
#5405 = CARTESIAN_POINT ( 'NONE',  ( -8.388197440586290909, -1.387539741535495974, 1.999999999999998224 ) ) ;
#5406 = CARTESIAN_POINT ( 'NONE',  ( 17.55913978494622896, -14.85518798308249266, -8.000000000000000000 ) ) ;
#5407 =( LENGTH_UNIT ( ) NAMED_UNIT ( * ) SI_UNIT ( .MILLI., .METRE. ) );
#5408 = CARTESIAN_POINT ( 'NONE',  ( 3.173694703385744997, 5.505084763670540227, 1.999999999999998224 ) ) ;
#5409 = ORIENTED_EDGE ( 'NONE', *, *, #3580, .F. ) ;
#5410 = CARTESIAN_POINT ( 'NONE',  ( 7.320916985966518631, 1.587212364775676843, 1.999999999999998224 ) ) ;
#5411 = CARTESIAN_POINT ( 'NONE',  ( 0.000000000000000000, 0.000000000000000000, -2.000000000000000000 ) ) ;
#5412 = FACE_OUTER_BOUND ( 'NONE', #3432, .T. ) ;
#5413 = CARTESIAN_POINT ( 'NONE',  ( 0.000000000000000000, 0.000000000000000000, 0.000000000000000000 ) ) ;
#5414 = APPLICATION_CONTEXT ( 'automotive_design' ) ;
#5415 = DIRECTION ( 'NONE',  ( -1.000000000000000000, 0.000000000000000000, 0.000000000000000000 ) ) ;
#5416 = DIRECTION ( 'NONE',  ( 0.000000000000000000, 0.000000000000000000, 1.000000000000000000 ) ) ;
#5417 = VERTEX_POINT ( 'NONE', #2957 ) ;
#5418 = DIRECTION ( 'NONE',  ( -0.000000000000000000, -0.000000000000000000, 1.000000000000000000 ) ) ;
#5419 = CARTESIAN_POINT ( 'NONE',  ( -7.559400777704423646, -6.425066744314204215, 14.00000000000000000 ) ) ;
#5420 = CARTESIAN_POINT ( 'NONE',  ( -7.091148812992122963, -4.571561645352110403, 1.999999999999998224 ) ) ;
#5421 = CARTESIAN_POINT ( 'NONE',  ( 7.990059919442647818, -3.149571442993177595, 1.999999999999998224 ) ) ;
#5422 = CARTESIAN_POINT ( 'NONE',  ( -1.515482495401828000, 9.129776367295956874, 14.00000000000000000 ) ) ;
#5423 = ORIENTED_EDGE ( 'NONE', *, *, #4598, .F. ) ;
#5424 = CARTESIAN_POINT ( 'NONE',  ( 22.00000000000000000, 0.000000000000000000, 4.000000000000001776 ) ) ;
#5425 = EDGE_CURVE ( 'NONE', #3518, #4802, #1638, .T. ) ;
#5426 = CARTESIAN_POINT ( 'NONE',  ( -3.987231204388229422, 4.693390172674912542, 13.99999999999953104 ) ) ;
#5427 = CARTESIAN_POINT ( 'NONE',  ( 1.870926337630180569, -8.025887876971657064, 13.99999999999999645 ) ) ;
#5428 = ADVANCED_FACE ( 'NONE', ( #1577 ), #1605, .T. ) ;
#5429 = CARTESIAN_POINT ( 'NONE',  ( -9.273719170356997665, -3.669762015052091098, 1.999999999999998224 ) ) ;
#5430 = ORIENTED_EDGE ( 'NONE', *, *, #3227, .F. ) ;
#5431 = CARTESIAN_POINT ( 'NONE',  ( -4.060726170632605658, -7.305992298388374273, 1.999999999999998224 ) ) ;
#5432 = DIRECTION ( 'NONE',  ( 0.000000000000000000, 0.000000000000000000, -1.000000000000000000 ) ) ;
#5433 = CARTESIAN_POINT ( 'NONE',  ( -2.547213823411294431, 6.752160688201485073, 1.999999999999998224 ) ) ;
#5434 = ORIENTED_EDGE ( 'NONE', *, *, #3787, .T. ) ;
#5435 = CARTESIAN_POINT ( 'NONE',  ( 2.161943361801394570, -6.363123982928429179, 1.999999999999998224 ) ) ;
#5436 = DIRECTION ( 'NONE',  ( -0.000000000000000000, -1.000000000000000000, -0.000000000000000000 ) ) ;
#5437 = CARTESIAN_POINT ( 'NONE',  ( 6.000000000000001776, 0.000000000000000000, 13.99999999999999645 ) ) ;
#5438 = ADVANCED_FACE ( 'NONE', ( #278 ), #302, .F. ) ;
#5439 = DIRECTION ( 'NONE',  ( 0.000000000000000000, 0.000000000000000000, 1.000000000000000000 ) ) ;
#5440 = CARTESIAN_POINT ( 'NONE',  ( 12.50000000000000000, 1.530808498934191521E-15, 14.00000000000000000 ) ) ;
#5441 = VERTEX_POINT ( 'NONE', #5576 ) ;
#5442 = CARTESIAN_POINT ( 'NONE',  ( -1.500000000000000444, 24.95495942693556302, 5.000000000000000000 ) ) ;
#5443 =( GEOMETRIC_REPRESENTATION_CONTEXT ( 3 ) GLOBAL_UNCERTAINTY_ASSIGNED_CONTEXT ( ( #1255 ) ) GLOBAL_UNIT_ASSIGNED_CONTEXT ( ( #1086, #742, #1689 ) ) REPRESENTATION_CONTEXT ( 'NONE', 'WORKASPACE' ) );
#5444 = CARTESIAN_POINT ( 'NONE',  ( 0.000000000000000000, 0.000000000000000000, 14.00000000000000000 ) ) ;
#5445 = CARTESIAN_POINT ( 'NONE',  ( -4.060726170632605658, -7.305992298388374273, 1.999999999999998224 ) ) ;
#5446 = CARTESIAN_POINT ( 'NONE',  ( 9.527640065893086430, 0.1642265212908741445, 1.999999999999998224 ) ) ;
#5447 = AXIS2_PLACEMENT_3D ( 'NONE', #304, #2958, #338 ) ;
#5448 = CARTESIAN_POINT ( 'NONE',  ( -8.913799778910966864, 1.613954699392568859, 14.00000000000000000 ) ) ;
#5449 = CARTESIAN_POINT ( 'NONE',  ( 1.300000000000000044, 0.000000000000000000, 1.249999999999999778 ) ) ;
#5450 = ORIENTED_EDGE ( 'NONE', *, *, #2896, .T. ) ;
#5451 = DIRECTION ( 'NONE',  ( -1.000000000000000000, -0.000000000000000000, -0.000000000000000000 ) ) ;
#5452 = DIRECTION ( 'NONE',  ( 1.000000000000000000, 0.000000000000000000, 0.000000000000000000 ) ) ;
#5453 = CARTESIAN_POINT ( 'NONE',  ( -4.581738566658776435, -9.288989786611782762, 13.99999999999999645 ) ) ;
#5454 = EDGE_CURVE ( 'NONE', #2713, #5376, #3395, .T. ) ;
#5455 = CARTESIAN_POINT ( 'NONE',  ( 10.48651993945612126, 0.8648464362367445091, 1.999999999999998224 ) ) ;
#5456 = AXIS2_PLACEMENT_3D ( 'NONE', #1781, #545, #3170 ) ;
#5457 = EDGE_LOOP ( 'NONE', ( #325, #5074, #4008, #3767, #2911, #1146 ) ) ;
#5458 = CARTESIAN_POINT ( 'NONE',  ( -5.210352092881994857, -6.569156856910357334, 1.999999999999998224 ) ) ;
#5459 = AXIS2_PLACEMENT_3D ( 'NONE', #4848, #2576, #469 ) ;
#5460 = DIRECTION ( 'NONE',  ( -3.540989467475305966E-16, -1.000000000000000000, -0.000000000000000000 ) ) ;
#5461 = SURFACE_STYLE_USAGE ( .BOTH. , #4140 ) ;
#5462 = CARTESIAN_POINT ( 'NONE',  ( -6.048456868091350636, 0.8014113234715940504, 1.999999999999998224 ) ) ;
#5463 = ADVANCED_FACE ( 'NONE', ( #4706 ), #768, .T. ) ;
#5464 = ORIENTED_EDGE ( 'NONE', *, *, #2300, .F. ) ;
#5465 = CARTESIAN_POINT ( 'NONE',  ( -2.547213823411294431, 6.752160688201485073, 1.999999999999998224 ) ) ;
#5466 = AXIS2_PLACEMENT_3D ( 'NONE', #574, #175, #4208 ) ;
#5467 = PLANE ( 'NONE',  #990 ) ;
#5468 = AXIS2_PLACEMENT_3D ( 'NONE', #3776, #5474, #3347 ) ;
#5469 = CARTESIAN_POINT ( 'NONE',  ( 0.000000000000000000, 0.000000000000000000, 4.000000000000000000 ) ) ;
#5470 = FACE_OUTER_BOUND ( 'NONE', #3939, .T. ) ;
#5471 = ORIENTED_EDGE ( 'NONE', *, *, #5501, .F. ) ;
#5472 = VECTOR ( 'NONE', #4348, 1000.000000000000000 ) ;
#5473 = FACE_OUTER_BOUND ( 'NONE', #2898, .T. ) ;
#5474 = DIRECTION ( 'NONE',  ( -0.000000000000000000, -0.000000000000000000, 1.000000000000000000 ) ) ;
#5475 = CARTESIAN_POINT ( 'NONE',  ( 1.870926337630253622, -8.025887876971653512, 1.999999999999998224 ) ) ;
#5476 = CARTESIAN_POINT ( 'NONE',  ( 1.870926337630180569, -8.025887876971657064, 13.99999999999999645 ) ) ;
#5477 = AXIS2_PLACEMENT_3D ( 'NONE', #1645, #4775, #2589 ) ;
#5478 = CARTESIAN_POINT ( 'NONE',  ( -3.139313036748680563, 9.741172307226465321, 1.999999999999998224 ) ) ;
#5479 = DIRECTION ( 'NONE',  ( -1.000000000000000000, -0.000000000000000000, -0.000000000000000000 ) ) ;
#5480 = EDGE_LOOP ( 'NONE', ( #4948, #2658, #427, #5019 ) ) ;
#5481 = FACE_OUTER_BOUND ( 'NONE', #501, .T. ) ;
#5482 = ORIENTED_EDGE ( 'NONE', *, *, #2032, .T. ) ;
#5483 = LINE ( 'NONE', #2340, #4744 ) ;
#5484 = CARTESIAN_POINT ( 'NONE',  ( -7.019001384594682591, 0.4577903460187995877, 14.00000000000000000 ) ) ;
#5485 = CARTESIAN_POINT ( 'NONE',  ( -3.127066335681350395, 9.214240776398044730, 13.99999999999999645 ) ) ;
#5486 = VECTOR ( 'NONE', #982, 1000.000000000000000 ) ;
#5487 = CARTESIAN_POINT ( 'NONE',  ( 6.452733273992156349, 8.145031704320794930, 1.999999999999998224 ) ) ;
#5488=STYLED_ITEM('',(#5730),#698);
#5489 = ORIENTED_EDGE ( 'NONE', *, *, #748, .F. ) ;
#5490 = CARTESIAN_POINT ( 'NONE',  ( 5.099673838352487998, -8.834479793761566668, 1.999999999999998224 ) ) ;
#5491 = CIRCLE ( 'NONE', #4662, 2.199999999999999289 ) ;
#5492 = DIRECTION ( 'NONE',  ( -0.000000000000000000, -0.000000000000000000, -1.000000000000000000 ) ) ;
#5493 = CARTESIAN_POINT ( 'NONE',  ( 5.772253124442284111, -3.205917188174072230, 1.999999999999998224 ) ) ;
#5494 = VERTEX_POINT ( 'NONE', #3852 ) ;
#5495 = CIRCLE ( 'NONE', #1270, 23.00000000000000000 ) ;
#5496 = CARTESIAN_POINT ( 'NONE',  ( 2.369394374793902802, -7.353877281245869035, 1.999999999999998224 ) ) ;
#5497 = DIRECTION ( 'NONE',  ( 0.000000000000000000, 0.000000000000000000, 1.000000000000000000 ) ) ;
#5498 =( NAMED_UNIT ( * ) PLANE_ANGLE_UNIT ( ) SI_UNIT ( $, .RADIAN. ) );
#5499 = FACE_OUTER_BOUND ( 'NONE', #1965, .T. ) ;
#5500 = UNCERTAINTY_MEASURE_WITH_UNIT (LENGTH_MEASURE( 1.000000000000000082E-05 ), #5407, 'distance_accuracy_value', 'NONE');
#5501 = EDGE_CURVE ( 'NONE', #1333, #186, #1662, .T. ) ;
#5502 = CARTESIAN_POINT ( 'NONE',  ( 1.300000000000000044, 1.443375672974065216, 7.017607234860990640E-28 ) ) ;
#5503 = ORIENTED_EDGE ( 'NONE', *, *, #4059, .F. ) ;
#5504 = DIRECTION ( 'NONE',  ( 1.000000000000000000, 0.000000000000000000, 0.000000000000000000 ) ) ;
#5505 = CARTESIAN_POINT ( 'NONE',  ( 2.667884741302309681, 9.975564253400266423, 14.00000000000000000 ) ) ;
#5506 = CARTESIAN_POINT ( 'NONE',  ( -4.227552200850895225, 7.601683304540809871, 1.999999999999998224 ) ) ;
#5507 = CARTESIAN_POINT ( 'NONE',  ( 7.812003909081977504, 1.689803927524662797, 13.99999999999999645 ) ) ;
#5508 = FACE_OUTER_BOUND ( 'NONE', #870, .T. ) ;
#5509 = ORIENTED_EDGE ( 'NONE', *, *, #5090, .T. ) ;
#5510 = DIRECTION ( 'NONE',  ( -0.000000000000000000, 1.000000000000000000, -0.000000000000000000 ) ) ;
#5511 = EDGE_LOOP ( 'NONE', ( #1849, #3515, #3547, #5489 ) ) ;
#5512 = CARTESIAN_POINT ( 'NONE',  ( 0.000000000000000000, 0.000000000000000000, 2.798278761944885229 ) ) ;
#5513 = CARTESIAN_POINT ( 'NONE',  ( 4.062840028443491569, -5.287223670286397059, 14.00000000000000000 ) ) ;
#5514 = CARTESIAN_POINT ( 'NONE',  ( 9.807503887221459493, -2.283819133639753751, 13.99999999999999645 ) ) ;
#5515 = CARTESIAN_POINT ( 'NONE',  ( -6.065725208710916583, -3.376743199310593635, 14.00000000000000000 ) ) ;
#5516 = EDGE_LOOP ( 'NONE', ( #3926, #1155, #232, #1221, #5678, #3332, #2435, #5143 ) ) ;
#5517 = CARTESIAN_POINT ( 'NONE',  ( -8.745075223330342595, 3.959260399367897421, 1.999999999999998224 ) ) ;
#5518 = DIRECTION ( 'NONE',  ( 0.000000000000000000, 0.000000000000000000, -1.000000000000000000 ) ) ;
#5519 = DIRECTION ( 'NONE',  ( 1.000000000000000000, 0.000000000000000000, 0.000000000000000000 ) ) ;
#5520 = CARTESIAN_POINT ( 'NONE',  ( 6.941605245898607279, 2.746080019686067519, 1.999999999999998224 ) ) ;
#5521 = VERTEX_POINT ( 'NONE', #474 ) ;
#5522 = CARTESIAN_POINT ( 'NONE',  ( 0.9466184546083533657, 7.233353930637701268, 1.999999999999998224 ) ) ;
#5523 = CARTESIAN_POINT ( 'NONE',  ( 1.623707939105925702, -6.078451570951504124, 1.999999999999998224 ) ) ;
#5524 = CARTESIAN_POINT ( 'NONE',  ( -6.465640026559317022, 4.020973141382162552, 13.99999999999999645 ) ) ;
#5525 = APPLICATION_CONTEXT ( 'automotive_design' ) ;
#5526 = EDGE_CURVE ( 'NONE', #3324, #261, #2475, .T. ) ;
#5527 = EDGE_CURVE ( 'NONE', #403, #2920, #1509, .T. ) ;
#5528 = DIRECTION ( 'NONE',  ( -2.385244779468107388E-15, -1.000000000000000000, 0.000000000000000000 ) ) ;
#5529 = ORIENTED_EDGE ( 'NONE', *, *, #3132, .T. ) ;
#5530 = FACE_OUTER_BOUND ( 'NONE', #1132, .T. ) ;
#5531 = CARTESIAN_POINT ( 'NONE',  ( 9.925004466819306259, 3.374327561486830440, 14.00000000000000000 ) ) ;
#5532 = CARTESIAN_POINT ( 'NONE',  ( -8.126042061586874254, 2.755650963504471473, 1.999999999999998224 ) ) ;
#5533 = ADVANCED_FACE ( 'NONE', ( #924 ), #2679, .F. ) ;
#5534 = CARTESIAN_POINT ( 'NONE',  ( 7.761517335261691741, -2.213789340049631349, 13.99999999999999645 ) ) ;
#5535 = CARTESIAN_POINT ( 'NONE',  ( 0.000000000000000000, 0.000000000000000000, -8.000000000000000000 ) ) ;
#5536 = VERTEX_POINT ( 'NONE', #4894 ) ;
#5537 = DIRECTION ( 'NONE',  ( 0.000000000000000000, 0.000000000000000000, -1.000000000000000000 ) ) ;
#5538 =( GEOMETRIC_REPRESENTATION_CONTEXT ( 3 ) GLOBAL_UNCERTAINTY_ASSIGNED_CONTEXT ( ( #3568 ) ) GLOBAL_UNIT_ASSIGNED_CONTEXT ( ( #3995, #3247, #4083 ) ) REPRESENTATION_CONTEXT ( 'NONE', 'WORKASPACE' ) );
#5539 = ORIENTED_EDGE ( 'NONE', *, *, #1160, .T. ) ;
#5540 = DIRECTION ( 'NONE',  ( -1.000000000000000000, 0.000000000000000000, 0.000000000000000000 ) ) ;
#5541 = CARTESIAN_POINT ( 'NONE',  ( 3.247347166530789586, 6.590896817052466439, 14.00000000000000000 ) ) ;
#5542 = CARTESIAN_POINT ( 'NONE',  ( 5.933674912743042817, -6.989438080420771193, 13.99999999999999645 ) ) ;
#5543 = CARTESIAN_POINT ( 'NONE',  ( -7.019651866616807290, -0.1200674265790614287, 14.00000000000000000 ) ) ;
#5544 = VERTEX_POINT ( 'NONE', #954 ) ;
#5545 = CARTESIAN_POINT ( 'NONE',  ( 8.697835924490032511, 4.836984431370230375, 1.999999999999998224 ) ) ;
#5546 = EDGE_CURVE ( 'NONE', #2459, #5397, #522, .T. ) ;
#5547 = FACE_OUTER_BOUND ( 'NONE', #1391, .T. ) ;
#5548 = CIRCLE ( 'NONE', #2151, 27.00000000000000355 ) ;
#5549 = DIRECTION ( 'NONE',  ( 0.000000000000000000, 0.000000000000000000, 1.000000000000000000 ) ) ;
#5550 = CARTESIAN_POINT ( 'NONE',  ( 0.5385325299235221852, 8.270587056550796845, 1.999999999999998224 ) ) ;
#5551 = DIRECTION ( 'NONE',  ( 0.000000000000000000, 0.000000000000000000, 1.000000000000000000 ) ) ;
#5552 = CARTESIAN_POINT ( 'NONE',  ( 1.869626052002640648, 6.555486721476421863, 13.99999999999999645 ) ) ;
#5553 = CIRCLE ( 'NONE', #1142, 5.000000000000000000 ) ;
#5554 = VECTOR ( 'NONE', #5460, 1000.000000000000000 ) ;
#5555 = DIRECTION ( 'NONE',  ( 1.000000000000000000, 0.000000000000000000, 0.000000000000000000 ) ) ;
#5556 = FILL_AREA_STYLE_COLOUR ( '', #3816 ) ;
#5557 = ORIENTED_EDGE ( 'NONE', *, *, #3162, .T. ) ;
#5558 = DIRECTION ( 'NONE',  ( -0.000000000000000000, -0.000000000000000000, 1.000000000000000000 ) ) ;
#5559 = DIRECTION ( 'NONE',  ( 0.000000000000000000, 0.000000000000000000, 1.000000000000000000 ) ) ;
#5560 = CARTESIAN_POINT ( 'NONE',  ( -9.500632974892678106, -0.6255030753161154866, 1.999999999999998224 ) ) ;
#5561 = PRESENTATION_LAYER_ASSIGNMENT (  '', '', ( #1053 ) ) ;
#5562 = CARTESIAN_POINT ( 'NONE',  ( -9.026614039607444795, -2.903226997913483487, 13.99999999999999645 ) ) ;
#5563 = CARTESIAN_POINT ( 'NONE',  ( -6.708753103182797162, 7.642576097240647570, 14.00000000000000000 ) ) ;
#5565 = ORIENTED_EDGE ( 'NONE', *, *, #5029, .T. ) ;
#5564 = CIRCLE ( 'NONE', #144, 13.00000000000000178 ) ;
#5566 = DIRECTION ( 'NONE',  ( -1.000000000000000000, 0.000000000000000000, 0.000000000000000000 ) ) ;
#5567 = ORIENTED_EDGE ( 'NONE', *, *, #1343, .F. ) ;
#5568 = CARTESIAN_POINT ( 'NONE',  ( -4.999999999999999112, 24.49489742783178770, 4.000000000000000000 ) ) ;
#5569 = CARTESIAN_POINT ( 'NONE',  ( -7.019651866616807290, -0.1200674265790614287, 14.00000000000000000 ) ) ;
#5570 = CARTESIAN_POINT ( 'NONE',  ( 3.605080641953931853, -9.570177220922108319, 13.99999999999999645 ) ) ;
#5571 = AXIS2_PLACEMENT_3D ( 'NONE', #1238, #4713, #778 ) ;
#5572 = CARTESIAN_POINT ( 'NONE',  ( 3.621982275015807939, -5.614208739972780471, 14.00000000000000000 ) ) ;
#5573 = ORIENTED_EDGE ( 'NONE', *, *, #4011, .F. ) ;
#5574 = AXIS2_PLACEMENT_3D ( 'NONE', #5589, #1216, #349 ) ;
#5575 = CARTESIAN_POINT ( 'NONE',  ( 0.7976699882155456889, 9.763020831628287155, 1.999999999999998224 ) ) ;
#5576 = CARTESIAN_POINT ( 'NONE',  ( 21.75000000000000000, -3.307189138830739061, 12.00000000000000000 ) ) ;
#5577 = VECTOR ( 'NONE', #1481, 1000.000000000000000 ) ;
#5578 = CARTESIAN_POINT ( 'NONE',  ( 0.000000000000000000, 0.000000000000000000, 0.000000000000000000 ) ) ;
#5579 = CARTESIAN_POINT ( 'NONE',  ( 4.776808680784692562, 5.634249062854761014, 1.999999999999998224 ) ) ;
#5580 = CARTESIAN_POINT ( 'NONE',  ( -1.451466707715830973, -6.203196315423896934, 1.999999999999998224 ) ) ;
#5581 = AXIS2_PLACEMENT_3D ( 'NONE', #2429, #5540, #3670 ) ;
#5582 = CARTESIAN_POINT ( 'NONE',  ( -7.211577653563209900, 2.317451195016654975, 13.99999999999999645 ) ) ;
#5583 = CARTESIAN_POINT ( 'NONE',  ( 9.123540010895986541, -2.926742269086382908, 1.999999999999998224 ) ) ;
#5584 = VECTOR ( 'NONE', #141, 1000.000000000000000 ) ;
#5585 = DIRECTION ( 'NONE',  ( 1.000000000000000000, 0.000000000000000000, 0.000000000000000000 ) ) ;
#5586 = SURFACE_STYLE_USAGE ( .BOTH. , #1272 ) ;
#5587 = EDGE_LOOP ( 'NONE', ( #2184, #1531 ) ) ;
#5588 = EDGE_CURVE ( 'NONE', #286, #2807, #1493, .T. ) ;
#5589 = CARTESIAN_POINT ( 'NONE',  ( 1.820000000000000062, 0.000000000000000000, 0.000000000000000000 ) ) ;
#5590 = DIRECTION ( 'NONE',  ( 0.000000000000000000, 0.000000000000000000, 1.000000000000000000 ) ) ;
#5591 = CARTESIAN_POINT ( 'NONE',  ( -5.337360893036674270, -7.710592058383929803, 13.99999999999999645 ) ) ;
#5592 = CARTESIAN_POINT ( 'NONE',  ( 7.108868828250529681, 7.597268273415099138, 14.00000000000000000 ) ) ;
#5593 = VERTEX_POINT ( 'NONE', #2794 ) ;
#5594 = CYLINDRICAL_SURFACE ( 'NONE', #4734, 0.2500000000000002220 ) ;
#5595 = VERTEX_POINT ( 'NONE', #2448 ) ;
#5596 = LINE ( 'NONE', #2086, #717 ) ;
#5597 = CARTESIAN_POINT ( 'NONE',  ( -3.597458971453999954, 6.226096630968013912, 14.00000000000000000 ) ) ;
#5598 = CARTESIAN_POINT ( 'NONE',  ( -5.623512120026769701, -3.262381593762911258, 1.999999999999998224 ) ) ;
#5599 = EDGE_CURVE ( 'NONE', #841, #1550, #4088, .T. ) ;
#5600 = CARTESIAN_POINT ( 'NONE',  ( 5.648567055624232225, 4.800053419556652656, 14.00000000000000000 ) ) ;
#5601 = VERTEX_POINT ( 'NONE', #2825 ) ;
#5602 = CARTESIAN_POINT ( 'NONE',  ( 1.176163838800080574, -10.19826953922189539, 1.999999999999998224 ) ) ;
#5603 = ADVANCED_FACE ( 'NONE', ( #4147, #3205 ), #1445, .F. ) ;
#5604 = SPHERICAL_SURFACE ( 'NONE', #2433, 4.324969328314201888 ) ;
#5605 = CARTESIAN_POINT ( 'NONE',  ( 7.311638624438941747, 4.225618826270679307, 1.999999999999998224 ) ) ;
#5606 = CARTESIAN_POINT ( 'NONE',  ( -3.379911625893426308, -5.460782782531098611, 1.999999999999998224 ) ) ;
#5607 = CARTESIAN_POINT ( 'NONE',  ( -5.810612947750823487, -4.611264106266947493, 13.99999999999999645 ) ) ;
#5608 = CARTESIAN_POINT ( 'NONE',  ( -9.445900372709948201, 3.550092993115765871, 1.999999999999998224 ) ) ;
#5609 = DIRECTION ( 'NONE',  ( 0.000000000000000000, 0.000000000000000000, -1.000000000000000000 ) ) ;
#5610 = LINE ( 'NONE', #1671, #5387 ) ;
#5611 = ORIENTED_EDGE ( 'NONE', *, *, #695, .T. ) ;
#5612 = CARTESIAN_POINT ( 'NONE',  ( 0.000000000000000000, 0.000000000000000000, 8.000000000000000000 ) ) ;
#5613 = CARTESIAN_POINT ( 'NONE',  ( 0.000000000000000000, 0.000000000000000000, -3.106350832689629637 ) ) ;
#5614 = EDGE_CURVE ( 'NONE', #4336, #3721, #5036, .T. ) ;
#5615 = CARTESIAN_POINT ( 'NONE',  ( 8.859712399101631775, -1.914114158827161294, 13.99999999999999645 ) ) ;
#5616 = CARTESIAN_POINT ( 'NONE',  ( 23.00000000000000000, -2.168404344971008868E-16, 16.41957833606399930 ) ) ;
#5617 = VERTEX_POINT ( 'NONE', #3629 ) ;
#5618 = DIRECTION ( 'NONE',  ( -1.000000000000000000, 0.000000000000000000, 0.000000000000000000 ) ) ;
#5619 = ORIENTED_EDGE ( 'NONE', *, *, #2032, .F. ) ;
#5620 = CARTESIAN_POINT ( 'NONE',  ( -5.399999999999998579, 26.45448922205832787, 4.000000000000000000 ) ) ;
#5621 = CARTESIAN_POINT ( 'NONE',  ( 8.477027301005275461, -1.108685663976147318, 14.00000000000000000 ) ) ;
#5622 = CARTESIAN_POINT ( 'NONE',  ( 2.803319092186594474, 10.45862564946370021, 13.99999999999999645 ) ) ;
#5623 = PRODUCT_DEFINITION_CONTEXT ( 'detailed design', #1512, 'design' ) ;
#5624 = CARTESIAN_POINT ( 'NONE',  ( 17.55913978494622896, -14.85518798308249266, -4.000000000000000000 ) ) ;
#5625 = CARTESIAN_POINT ( 'NONE',  ( -5.395431796987672612, -5.765308706272596950, 14.00000000000000000 ) ) ;
#5626 = ORIENTED_EDGE ( 'NONE', *, *, #1083, .F. ) ;
#5627 = ADVANCED_FACE ( 'NONE', ( #3254 ), #2853, .T. ) ;
#5628 = LINE ( 'NONE', #1376, #1818 ) ;
#5629 = PRESENTATION_LAYER_ASSIGNMENT (  '', '', ( #1583 ) ) ;
#5630 = CARTESIAN_POINT ( 'NONE',  ( 21.75000000000000000, 2.891205793294679929E-17, 4.000000000000001776 ) ) ;
#5631 = SHAPE_REPRESENTATION_RELATIONSHIP ( 'NONE' , 'NONE' ,  #1362, #622 ) ;
#5632 =( REPRESENTATION_RELATIONSHIP ('NONE','NONE', #4854, #4116 ) REPRESENTATION_RELATIONSHIP_WITH_TRANSFORMATION ( #4422 )SHAPE_REPRESENTATION_RELATIONSHIP( ) );
#5633 = CARTESIAN_POINT ( 'NONE',  ( 0.5141566911143078400, -7.748312628312726602, 1.999999999999998224 ) ) ;
#5634 = CARTESIAN_POINT ( 'NONE',  ( 23.24999999999999645, -8.485281374238580199, 8.000000000000000000 ) ) ;
#5635 = CARTESIAN_POINT ( 'NONE',  ( -7.227555219266157849, -1.939125212622549999, 13.99999999999999645 ) ) ;
#5636 = CARTESIAN_POINT ( 'NONE',  ( 5.030817567586499450, 9.062633982223127660, 1.999999999999998224 ) ) ;
#5637 = FACE_BOUND ( 'NONE', #5278, .T. ) ;
#5638=STYLED_ITEM('',(#5716),#4482);
#5639 =( NAMED_UNIT ( * ) PLANE_ANGLE_UNIT ( ) SI_UNIT ( $, .RADIAN. ) );
#5640 = EDGE_LOOP ( 'NONE', ( #3781, #2812, #2076, #5224 ) ) ;
#5641 = DIRECTION ( 'NONE',  ( 0.000000000000000000, 0.000000000000000000, -1.000000000000000000 ) ) ;
#5642 = LINE ( 'NONE', #2565, #3720 ) ;
#5643 = AXIS2_PLACEMENT_3D ( 'NONE', #3208, #180, #2363 ) ;
#5644 = AXIS2_PLACEMENT_3D ( 'NONE', #4391, #2204, #3956 ) ;
#5645 = CARTESIAN_POINT ( 'NONE',  ( 0.5754137710878940437, 8.770917875152660415, 13.99999999999999645 ) ) ;
#5646 = PLANE ( 'NONE',  #582 ) ;
#5647 = VERTEX_POINT ( 'NONE', #664 ) ;
#5648 = DIRECTION ( 'NONE',  ( 1.000000000000000000, 0.000000000000000000, 0.000000000000000000 ) ) ;
#5649 = ORIENTED_EDGE ( 'NONE', *, *, #2544, .F. ) ;
#5650 = CARTESIAN_POINT ( 'NONE',  ( -2.000000000000000000, 2.449293598294706414E-16, 8.000000000000000000 ) ) ;
#5651 = AXIS2_PLACEMENT_3D ( 'NONE', #4486, #168, #1838 ) ;
#5652 = ADVANCED_FACE ( 'NONE', ( #5499 ), #4093, .T. ) ;
#5653 = CARTESIAN_POINT ( 'NONE',  ( -2.138212235155100061, 7.953261502403491612, 14.00000000000000000 ) ) ;
#5654 = CARTESIAN_POINT ( 'NONE',  ( -2.466819000628106551, 6.242838961510105200, 1.999999999999998224 ) ) ;
#5655 = MECHANICAL_DESIGN_GEOMETRIC_PRESENTATION_REPRESENTATION (  '', ( #3266 ), #4278 ) ;
#5656 = CARTESIAN_POINT ( 'NONE',  ( 0.000000000000000000, 0.000000000000000000, 4.000000000000000000 ) ) ;
#5657 = CARTESIAN_POINT ( 'NONE',  ( 8.156937663706065322, 2.333191796391004047, 14.00000000000000000 ) ) ;
#5658 = VERTEX_POINT ( 'NONE', #1527 ) ;
#5659 = FACE_OUTER_BOUND ( 'NONE', #1616, .T. ) ;
#5660 = AXIS2_PLACEMENT_3D ( 'NONE', #3809, #4189, #3754 ) ;
#5661 = CARTESIAN_POINT ( 'NONE',  ( -6.505530684480628878, -3.618119970335913038, 13.99999999999999645 ) ) ;
#5662 = EDGE_CURVE ( 'NONE', #4851, #5544, #5102, .T. ) ;
#5663 = CARTESIAN_POINT ( 'NONE',  ( -0.2798806129216870886, -8.779921314118375619, 1.999999999999998224 ) ) ;
#5664 = AXIS2_PLACEMENT_3D ( 'NONE', #4974, #2879, #2390 ) ;
#5665 = CARTESIAN_POINT ( 'NONE',  ( -1.189470317277863121, -7.202885406307536265, 1.999999999999998224 ) ) ;
#5666 = CARTESIAN_POINT ( 'NONE',  ( -0.1359230501496729582, -8.279147739301068398, 13.99999999999999645 ) ) ;
#5667 = DIRECTION ( 'NONE',  ( -3.540989467475305966E-16, -1.000000000000000000, 0.000000000000000000 ) ) ;
#5668 = DIRECTION ( 'NONE',  ( 1.000000000000000000, 0.000000000000000000, 0.000000000000000000 ) ) ;
#5669 = VECTOR ( 'NONE', #3927, 1000.000000000000000 ) ;
#5670 = DIRECTION ( 'NONE',  ( 0.000000000000000000, 0.000000000000000000, 1.000000000000000000 ) ) ;
#5671 = DIRECTION ( 'NONE',  ( 1.000000000000000000, 0.000000000000000000, 0.000000000000000000 ) ) ;
#5672 = ORIENTED_EDGE ( 'NONE', *, *, #4813, .F. ) ;
#5673 = CIRCLE ( 'NONE', #3285, 22.50000000000000355 ) ;
#5674 = CARTESIAN_POINT ( 'NONE',  ( -8.017392084630589721, -4.988806607527435766, 13.99999999999999645 ) ) ;
#5675 = ADVANCED_FACE ( 'NONE', ( #1121 ), #3085, .T. ) ;
#5676 = LINE ( 'NONE', #3864, #3343 ) ;
#5677 = EDGE_CURVE ( 'NONE', #3244, #1117, #145, .T. ) ;
#5678 = ORIENTED_EDGE ( 'NONE', *, *, #3752, .T. ) ;
#5679 = DIRECTION ( 'NONE',  ( -0.2000000000000004274, -0.9797958971132710859, 0.000000000000000000 ) ) ;
#5680 = EDGE_LOOP ( 'NONE', ( #3573, #109 ) ) ;
#5681 = CARTESIAN_POINT ( 'NONE',  ( 2.400000000000000799, 2.694222958124176020E-16, -2.199999999999999289 ) ) ;
#5682 = CARTESIAN_POINT ( 'NONE',  ( -4.424777426322135554, -7.679192617324877901, 14.00000000000000000 ) ) ;
#5683 = CARTESIAN_POINT ( 'NONE',  ( -10.48421140591525713, 1.206973991593908169, 13.99999999999999645 ) ) ;
#5684 = DIRECTION ( 'NONE',  ( 1.000000000000000000, 4.364351673553916694E-15, 0.000000000000000000 ) ) ;
#5685 = CARTESIAN_POINT ( 'NONE',  ( 6.591354251721611490, -5.587324598951901145, 14.00000000000000000 ) ) ;
#5686 = VERTEX_POINT ( 'NONE', #4952 ) ;
#5687 = DIRECTION ( 'NONE',  ( -0.000000000000000000, -0.000000000000000000, -1.000000000000000000 ) ) ;
#5688 = DIRECTION ( 'NONE',  ( 1.000000000000000000, 0.000000000000000000, 0.000000000000000000 ) ) ;
#5689 = NEXT_ASSEMBLY_USAGE_OCCURRENCE ( 'NAUO1', ' ', ' ', #5209, #2040, $ ) ;
#5690 = NEXT_ASSEMBLY_USAGE_OCCURRENCE ( 'NAUO2', ' ', ' ', #5209, #1447, $ ) ;
#5691 = NEXT_ASSEMBLY_USAGE_OCCURRENCE ( 'NAUO3', ' ', ' ', #5209, #3907, $ ) ;
#5692 = NEXT_ASSEMBLY_USAGE_OCCURRENCE ( 'NAUO4', ' ', ' ', #5209, #4780, $ ) ;
#5693 = NEXT_ASSEMBLY_USAGE_OCCURRENCE ( 'NAUO5', ' ', ' ', #5209, #177, $ ) ;
#5694 = NEXT_ASSEMBLY_USAGE_OCCURRENCE ( 'NAUO6', ' ', ' ', #5209, #4858, $ ) ;
#5695 = NEXT_ASSEMBLY_USAGE_OCCURRENCE ( 'NAUO7', ' ', ' ', #5209, #3839, $ ) ;
#5696=COLOUR_RGB('Dark Blue',0.08,0.2,0.34);
#5697=FILL_AREA_STYLE_COLOUR('',#5696);
#5698=FILL_AREA_STYLE('',(#5697));
#5699=SURFACE_STYLE_FILL_AREA(#5698);
#5700=SURFACE_SIDE_STYLE('',(#5699));
#5701=SURFACE_STYLE_USAGE(.BOTH.,#5700);
#5702=PRESENTATION_STYLE_ASSIGNMENT((#5701));
#5703=COLOUR_RGB('Light Blue',0.38,0.62,0.78);
#5704=FILL_AREA_STYLE_COLOUR('',#5703);
#5705=FILL_AREA_STYLE('',(#5704));
#5706=SURFACE_STYLE_FILL_AREA(#5705);
#5707=SURFACE_SIDE_STYLE('',(#5706));
#5708=SURFACE_STYLE_USAGE(.BOTH.,#5707);
#5709=PRESENTATION_STYLE_ASSIGNMENT((#5708));
#5710=COLOUR_RGB('Sky Blue',0.24,0.69,0.87);
#5711=FILL_AREA_STYLE_COLOUR('',#5710);
#5712=FILL_AREA_STYLE('',(#5711));
#5713=SURFACE_STYLE_FILL_AREA(#5712);
#5714=SURFACE_SIDE_STYLE('',(#5713));
#5715=SURFACE_STYLE_USAGE(.BOTH.,#5714);
#5716=PRESENTATION_STYLE_ASSIGNMENT((#5715));
#5717=COLOUR_RGB('Grey',0.48,0.52,0.57);
#5718=FILL_AREA_STYLE_COLOUR('',#5717);
#5719=FILL_AREA_STYLE('',(#5718));
#5720=SURFACE_STYLE_FILL_AREA(#5719);
#5721=SURFACE_SIDE_STYLE('',(#5720));
#5722=SURFACE_STYLE_USAGE(.BOTH.,#5721);
#5723=PRESENTATION_STYLE_ASSIGNMENT((#5722));
#5724=COLOUR_RGB('Black',0.12,0.14,0.17);
#5725=FILL_AREA_STYLE_COLOUR('',#5724);
#5726=FILL_AREA_STYLE('',(#5725));
#5727=SURFACE_STYLE_FILL_AREA(#5726);
#5728=SURFACE_SIDE_STYLE('',(#5727));
#5729=SURFACE_STYLE_USAGE(.BOTH.,#5728);
#5730=PRESENTATION_STYLE_ASSIGNMENT((#5729));
#5731=COLOUR_RGB('Off White',0.89,0.88,0.83);
#5732=FILL_AREA_STYLE_COLOUR('',#5731);
#5733=FILL_AREA_STYLE('',(#5732));
#5734=SURFACE_STYLE_FILL_AREA(#5733);
#5735=SURFACE_SIDE_STYLE('',(#5734));
#5736=SURFACE_STYLE_USAGE(.BOTH.,#5735);
#5737=PRESENTATION_STYLE_ASSIGNMENT((#5736));
ENDSEC;
END-ISO-10303-21;
